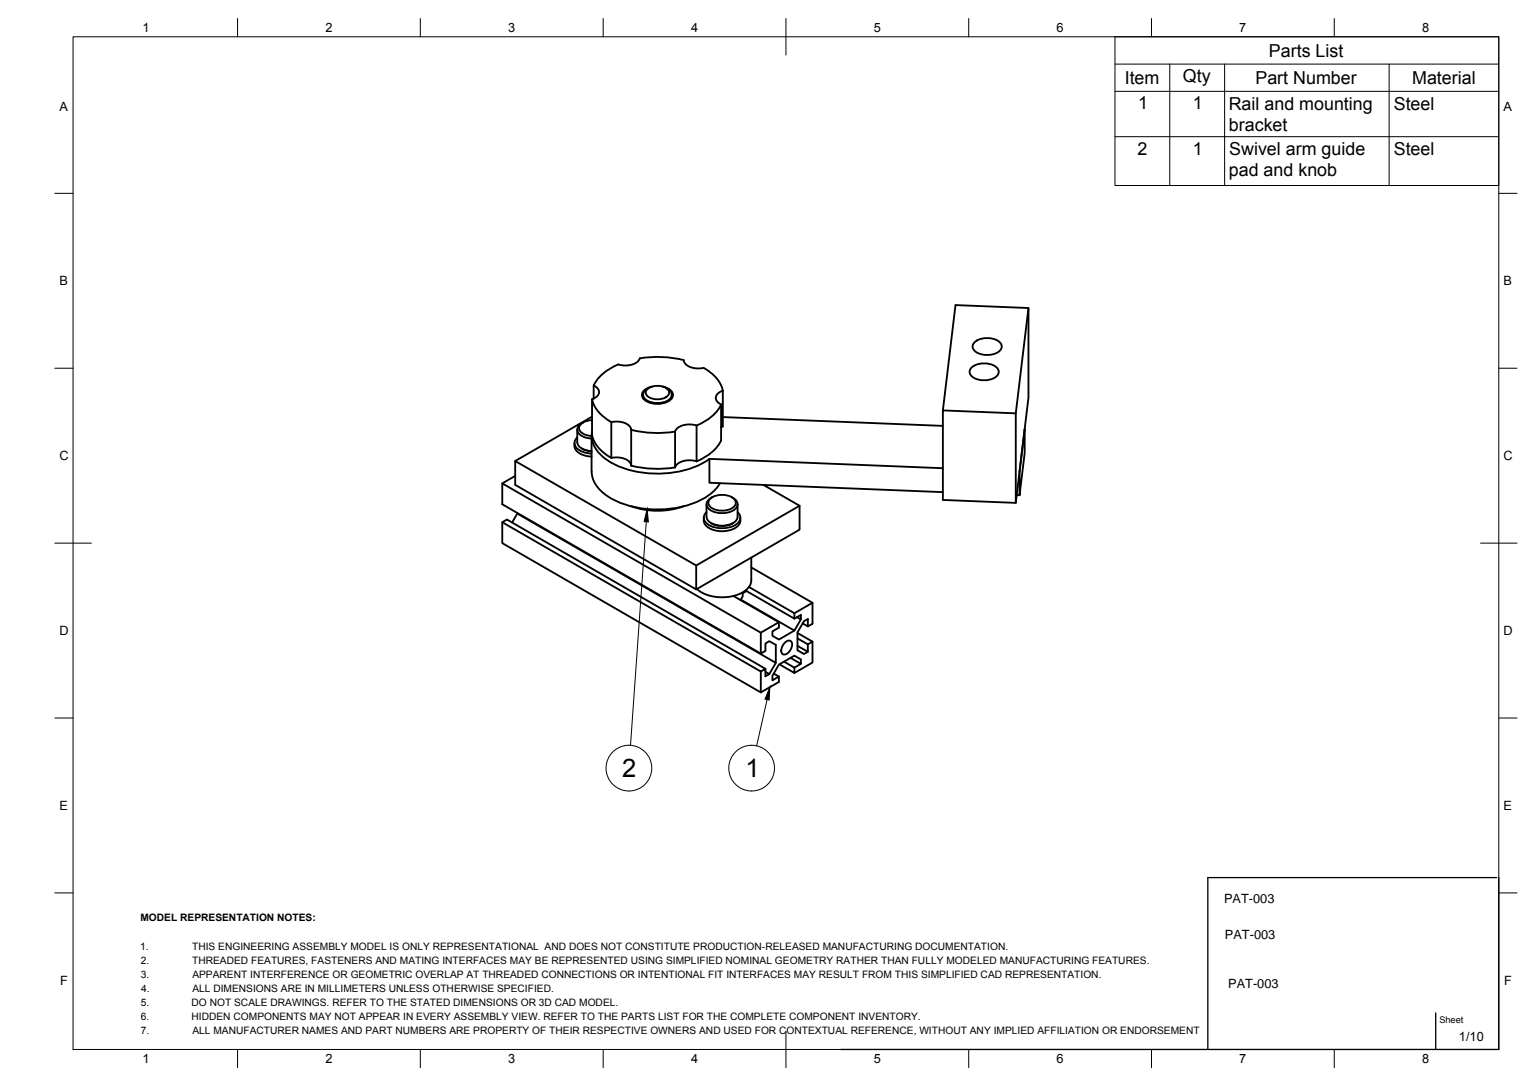
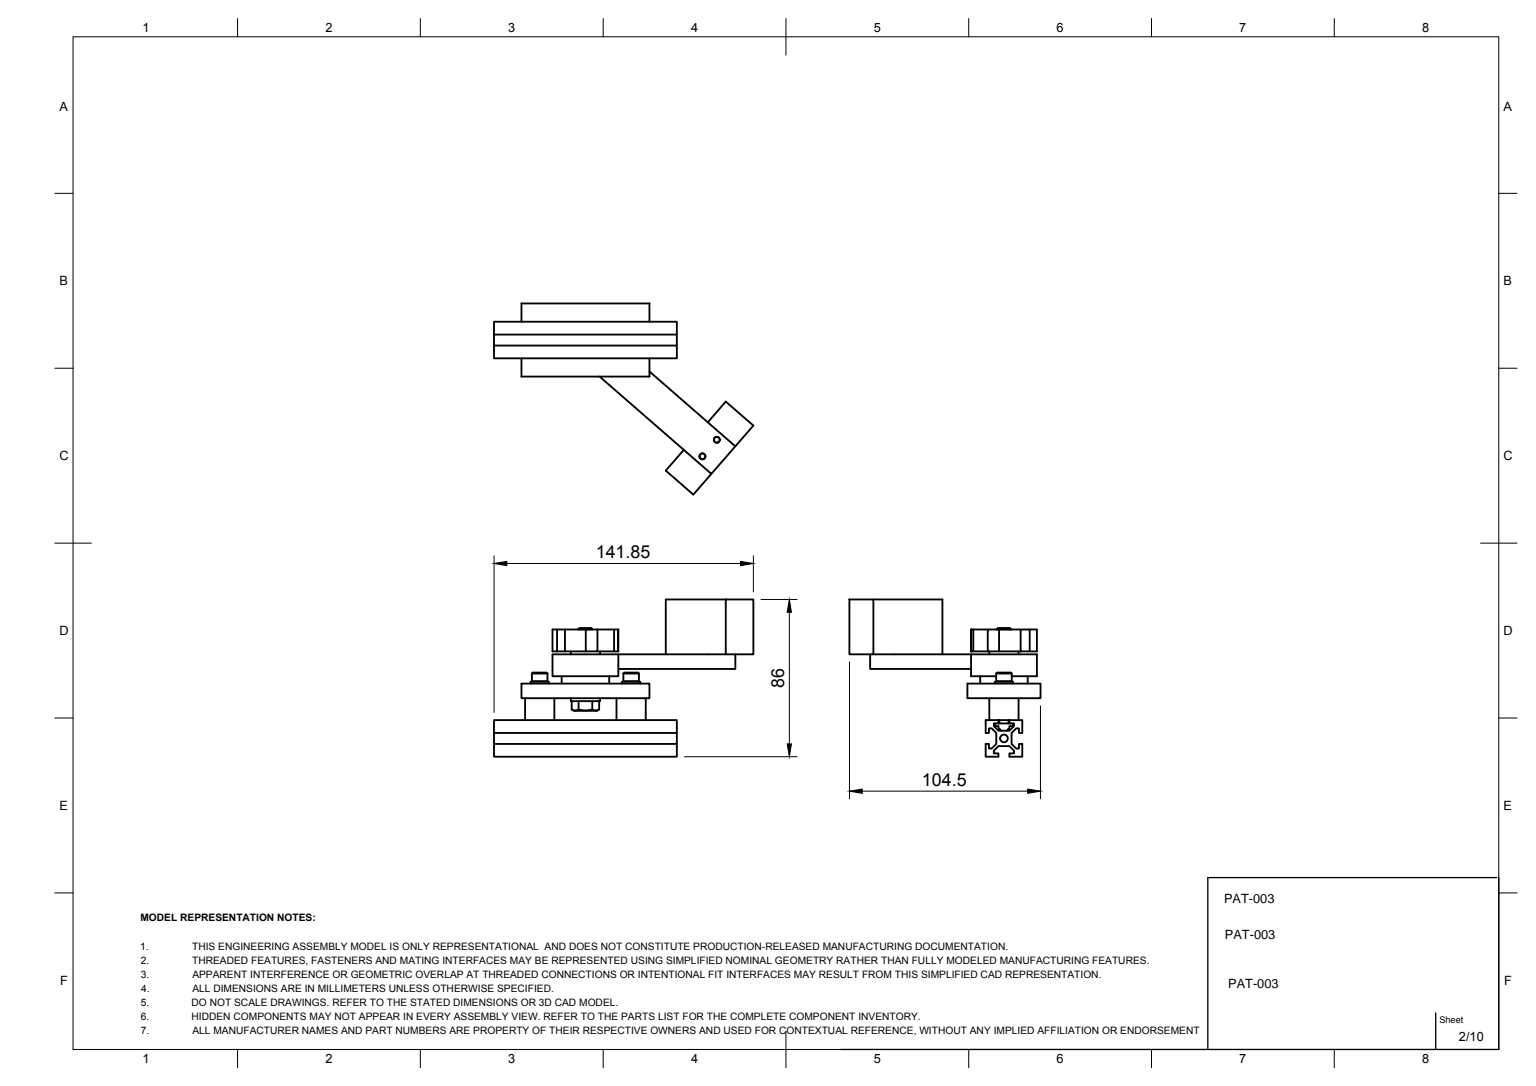
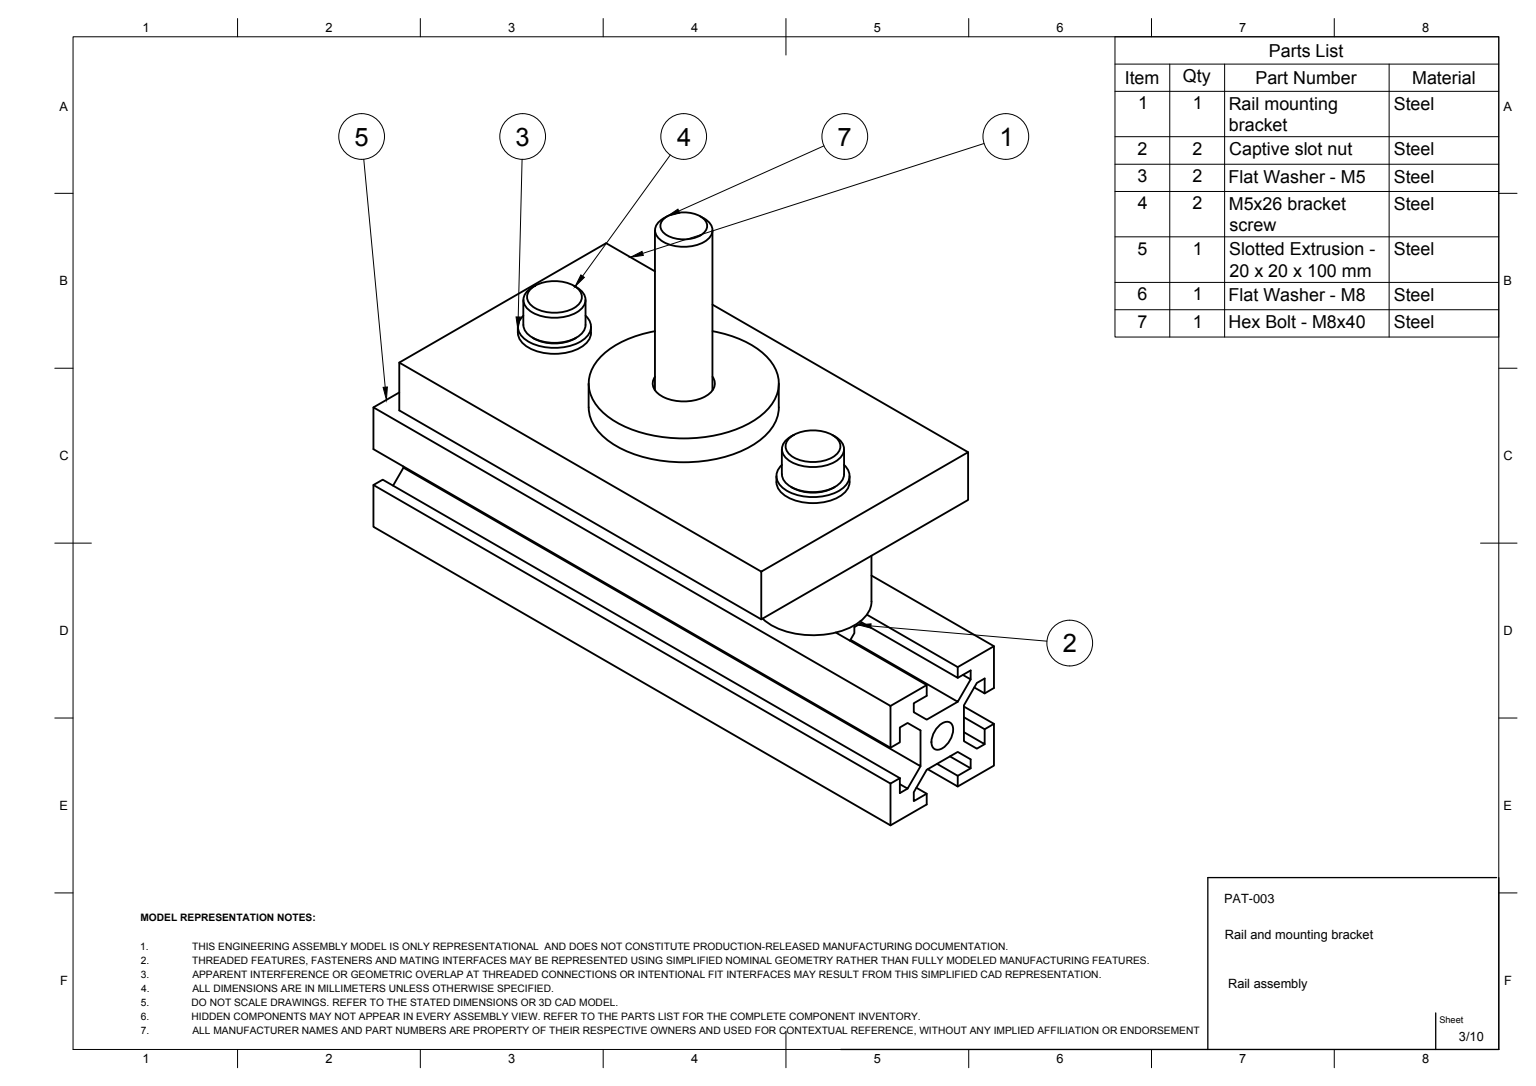
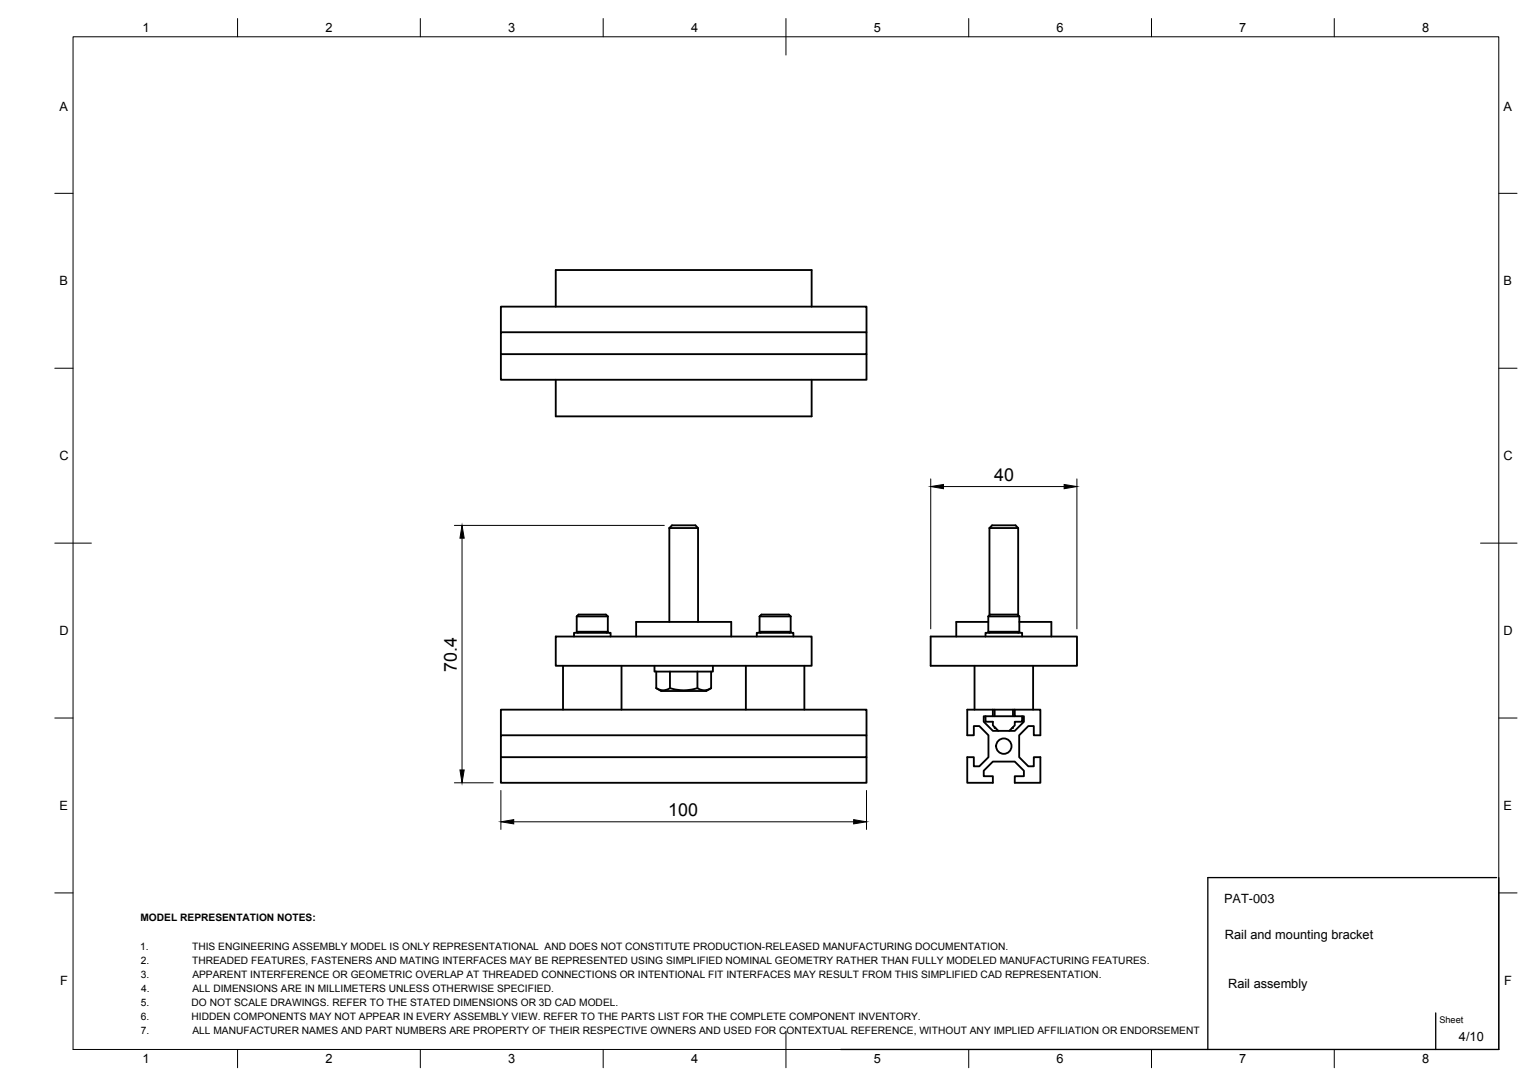
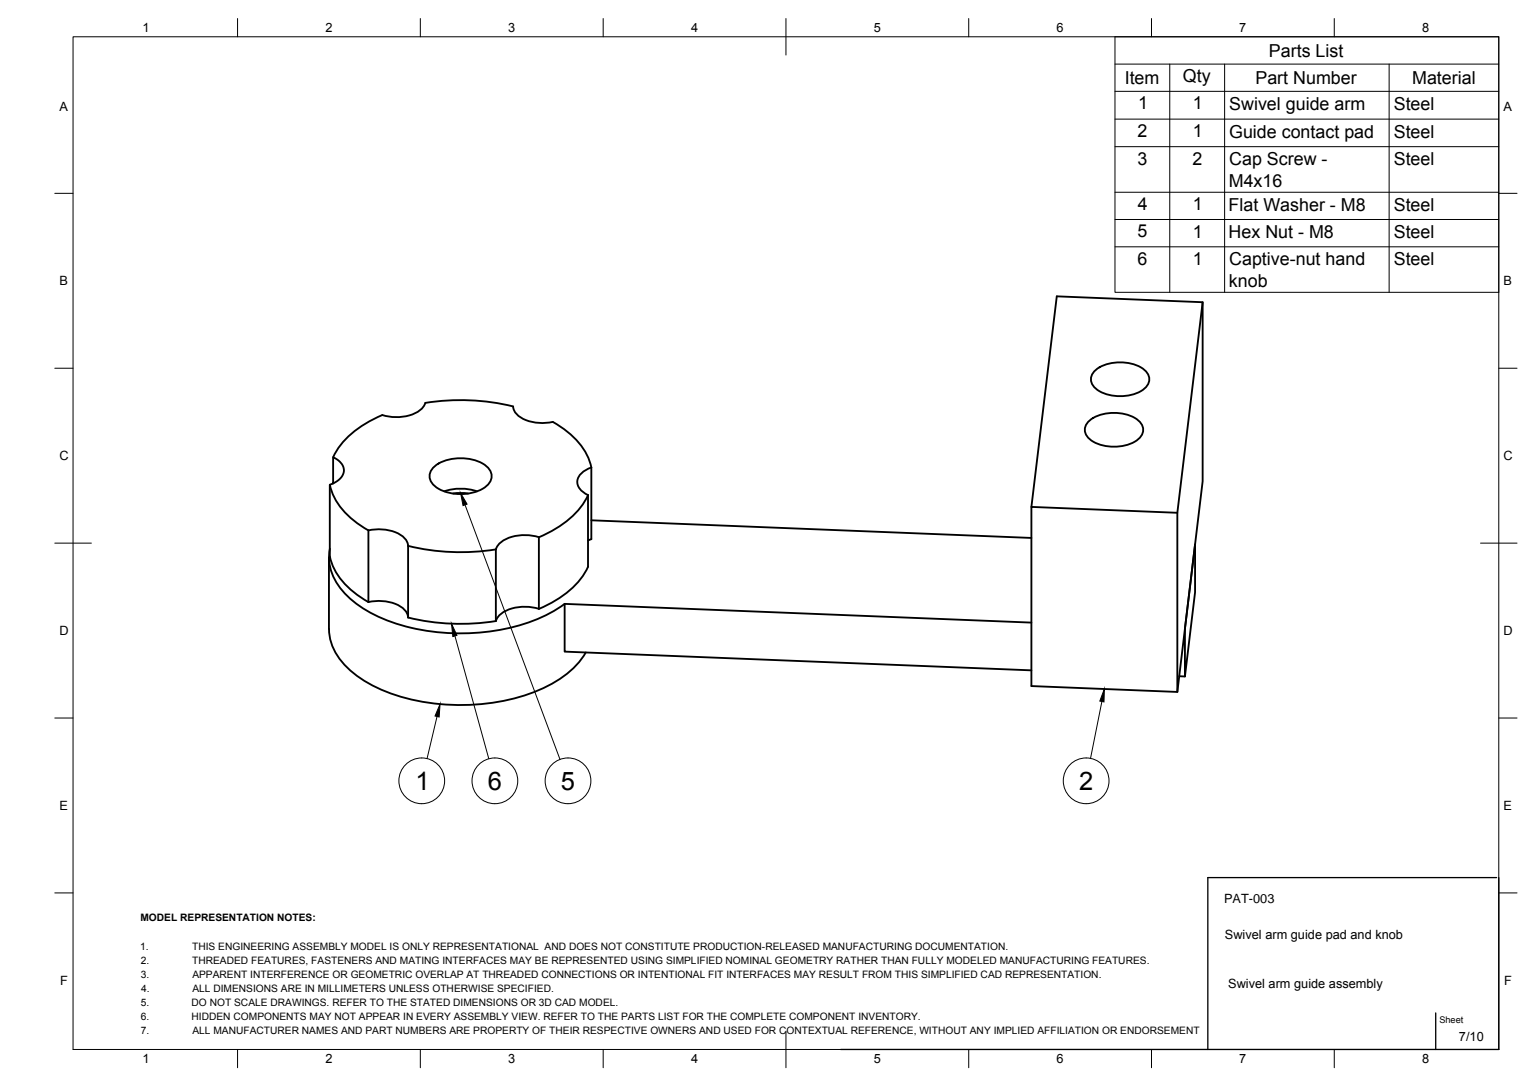
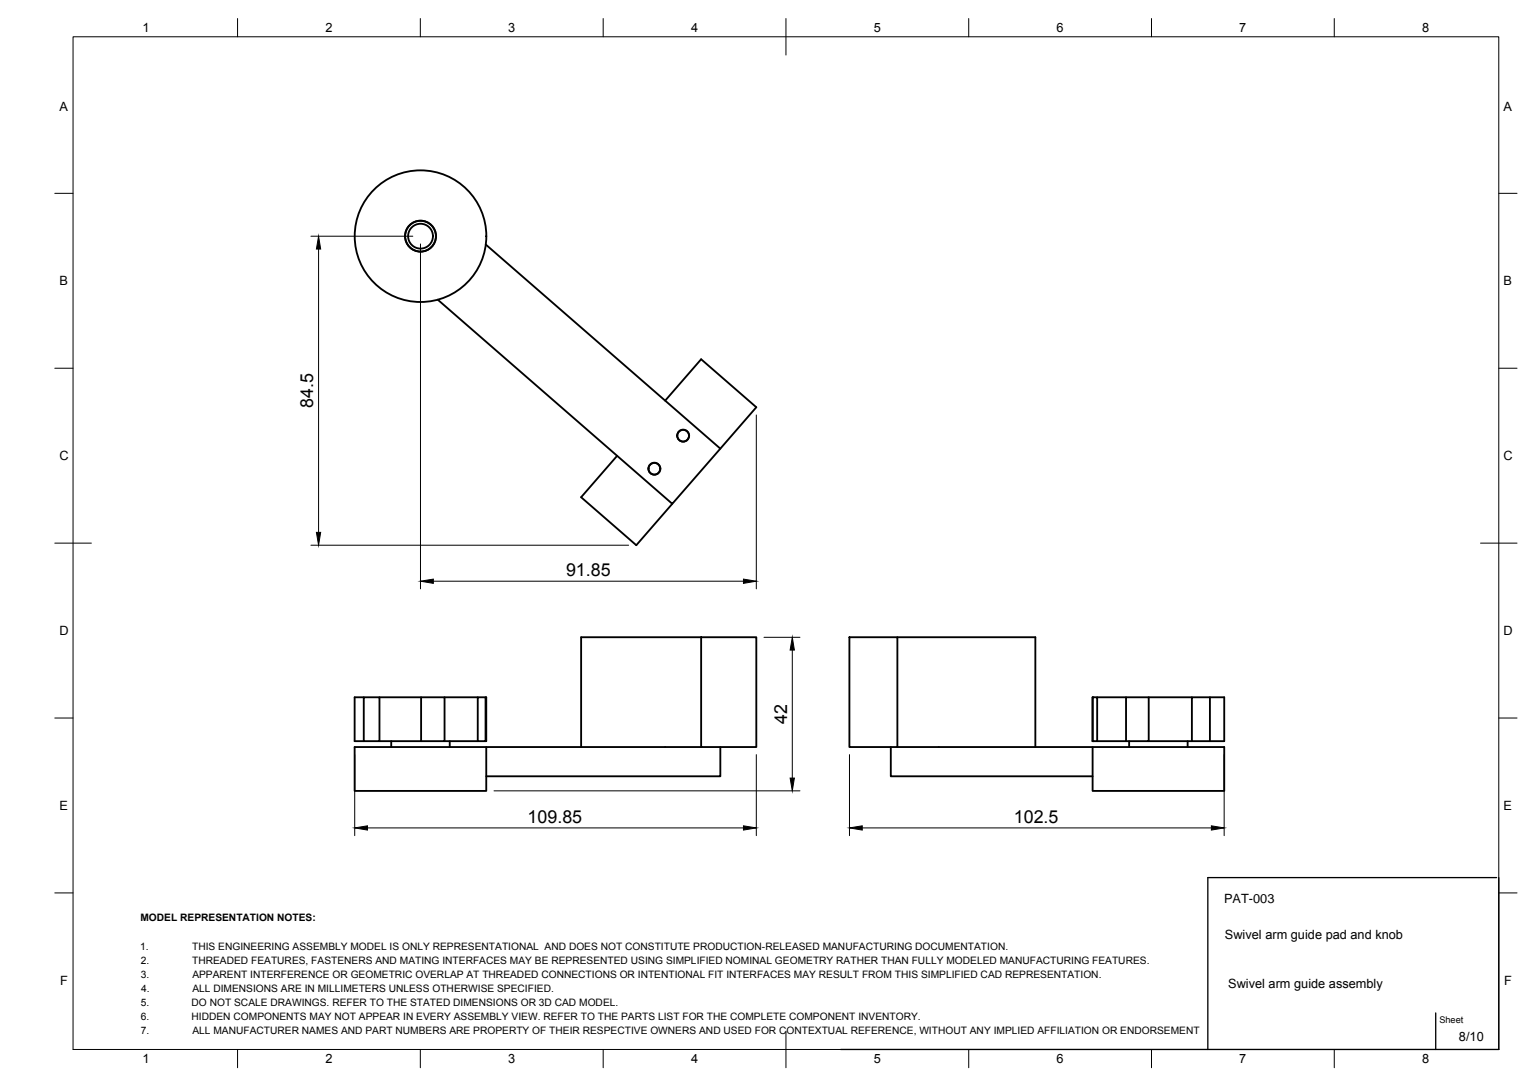
ISO-10303-21;
HEADER;
/* Generated by software containing ST-Developer
 * from STEP Tools, Inc. (www.steptools.com) 
 */

FILE_DESCRIPTION(
/* description */ ('PAT-003'),
/* implementation_level */ '2;1');

FILE_NAME(
/* name */ 'PAT-003',
/* time_stamp */ '2026-10-29T15:45:40-07:00',
/* author */ (''),
/* organization */ (''),
/* preprocessor_version */ 'ST-DEVELOPER v20.2',
/* originating_system */ 'Autodesk Translation Framework v15.17.0.0',
/* authorisation */ '');

FILE_SCHEMA (('AUTOMOTIVE_DESIGN { 1 0 10303 214 3 1 1 }'));
ENDSEC;

DATA;
#10=MECHANICAL_DESIGN_GEOMETRIC_PRESENTATION_REPRESENTATION('',(#147,#148,
#149,#150,#151,#152,#153,#154,#155,#156,#157,#158),#5761);
#11=ITEM_DEFINED_TRANSFORMATION($,$,#3470,#3703);
#12=ITEM_DEFINED_TRANSFORMATION($,$,#3498,#3704);
#13=ITEM_DEFINED_TRANSFORMATION($,$,#3519,#3705);
#14=ITEM_DEFINED_TRANSFORMATION($,$,#3530,#3706);
#15=ITEM_DEFINED_TRANSFORMATION($,$,#3498,#3707);
#16=ITEM_DEFINED_TRANSFORMATION($,$,#3519,#3708);
#17=ITEM_DEFINED_TRANSFORMATION($,$,#3530,#3709);
#18=ITEM_DEFINED_TRANSFORMATION($,$,#3558,#3710);
#19=ITEM_DEFINED_TRANSFORMATION($,$,#3694,#3711);
#20=ITEM_DEFINED_TRANSFORMATION($,$,#3608,#3712);
#21=ITEM_DEFINED_TRANSFORMATION($,$,#3626,#3778);
#22=ITEM_DEFINED_TRANSFORMATION($,$,#3647,#3779);
#23=ITEM_DEFINED_TRANSFORMATION($,$,#3668,#3780);
#24=ITEM_DEFINED_TRANSFORMATION($,$,#3668,#3781);
#25=ITEM_DEFINED_TRANSFORMATION($,$,#3694,#3782);
#26=ITEM_DEFINED_TRANSFORMATION($,$,#3713,#3783);
#27=ITEM_DEFINED_TRANSFORMATION($,$,#3729,#3784);
#28=ITEM_DEFINED_TRANSFORMATION($,$,#3469,#3785);
#29=ITEM_DEFINED_TRANSFORMATION($,$,#3625,#3786);
#30=(
REPRESENTATION_RELATIONSHIP($,$,#5817,#5816)
REPRESENTATION_RELATIONSHIP_WITH_TRANSFORMATION(#11)
SHAPE_REPRESENTATION_RELATIONSHIP()
);
#31=(
REPRESENTATION_RELATIONSHIP($,$,#5818,#5816)
REPRESENTATION_RELATIONSHIP_WITH_TRANSFORMATION(#12)
SHAPE_REPRESENTATION_RELATIONSHIP()
);
#32=(
REPRESENTATION_RELATIONSHIP($,$,#5819,#5816)
REPRESENTATION_RELATIONSHIP_WITH_TRANSFORMATION(#13)
SHAPE_REPRESENTATION_RELATIONSHIP()
);
#33=(
REPRESENTATION_RELATIONSHIP($,$,#5820,#5816)
REPRESENTATION_RELATIONSHIP_WITH_TRANSFORMATION(#14)
SHAPE_REPRESENTATION_RELATIONSHIP()
);
#34=(
REPRESENTATION_RELATIONSHIP($,$,#5818,#5816)
REPRESENTATION_RELATIONSHIP_WITH_TRANSFORMATION(#15)
SHAPE_REPRESENTATION_RELATIONSHIP()
);
#35=(
REPRESENTATION_RELATIONSHIP($,$,#5819,#5816)
REPRESENTATION_RELATIONSHIP_WITH_TRANSFORMATION(#16)
SHAPE_REPRESENTATION_RELATIONSHIP()
);
#36=(
REPRESENTATION_RELATIONSHIP($,$,#5820,#5816)
REPRESENTATION_RELATIONSHIP_WITH_TRANSFORMATION(#17)
SHAPE_REPRESENTATION_RELATIONSHIP()
);
#37=(
REPRESENTATION_RELATIONSHIP($,$,#5821,#5816)
REPRESENTATION_RELATIONSHIP_WITH_TRANSFORMATION(#18)
SHAPE_REPRESENTATION_RELATIONSHIP()
);
#38=(
REPRESENTATION_RELATIONSHIP($,$,#5827,#5816)
REPRESENTATION_RELATIONSHIP_WITH_TRANSFORMATION(#19)
SHAPE_REPRESENTATION_RELATIONSHIP()
);
#39=(
REPRESENTATION_RELATIONSHIP($,$,#5822,#5816)
REPRESENTATION_RELATIONSHIP_WITH_TRANSFORMATION(#20)
SHAPE_REPRESENTATION_RELATIONSHIP()
);
#40=(
REPRESENTATION_RELATIONSHIP($,$,#5824,#5823)
REPRESENTATION_RELATIONSHIP_WITH_TRANSFORMATION(#21)
SHAPE_REPRESENTATION_RELATIONSHIP()
);
#41=(
REPRESENTATION_RELATIONSHIP($,$,#5825,#5823)
REPRESENTATION_RELATIONSHIP_WITH_TRANSFORMATION(#22)
SHAPE_REPRESENTATION_RELATIONSHIP()
);
#42=(
REPRESENTATION_RELATIONSHIP($,$,#5826,#5823)
REPRESENTATION_RELATIONSHIP_WITH_TRANSFORMATION(#23)
SHAPE_REPRESENTATION_RELATIONSHIP()
);
#43=(
REPRESENTATION_RELATIONSHIP($,$,#5826,#5823)
REPRESENTATION_RELATIONSHIP_WITH_TRANSFORMATION(#24)
SHAPE_REPRESENTATION_RELATIONSHIP()
);
#44=(
REPRESENTATION_RELATIONSHIP($,$,#5827,#5823)
REPRESENTATION_RELATIONSHIP_WITH_TRANSFORMATION(#25)
SHAPE_REPRESENTATION_RELATIONSHIP()
);
#45=(
REPRESENTATION_RELATIONSHIP($,$,#5828,#5823)
REPRESENTATION_RELATIONSHIP_WITH_TRANSFORMATION(#26)
SHAPE_REPRESENTATION_RELATIONSHIP()
);
#46=(
REPRESENTATION_RELATIONSHIP($,$,#5829,#5823)
REPRESENTATION_RELATIONSHIP_WITH_TRANSFORMATION(#27)
SHAPE_REPRESENTATION_RELATIONSHIP()
);
#47=(
REPRESENTATION_RELATIONSHIP($,$,#5816,#5815)
REPRESENTATION_RELATIONSHIP_WITH_TRANSFORMATION(#28)
SHAPE_REPRESENTATION_RELATIONSHIP()
);
#48=(
REPRESENTATION_RELATIONSHIP($,$,#5823,#5815)
REPRESENTATION_RELATIONSHIP_WITH_TRANSFORMATION(#29)
SHAPE_REPRESENTATION_RELATIONSHIP()
);
#49=CONTEXT_DEPENDENT_SHAPE_REPRESENTATION(#30,#5794);
#50=CONTEXT_DEPENDENT_SHAPE_REPRESENTATION(#31,#5795);
#51=CONTEXT_DEPENDENT_SHAPE_REPRESENTATION(#32,#5796);
#52=CONTEXT_DEPENDENT_SHAPE_REPRESENTATION(#33,#5797);
#53=CONTEXT_DEPENDENT_SHAPE_REPRESENTATION(#34,#5798);
#54=CONTEXT_DEPENDENT_SHAPE_REPRESENTATION(#35,#5799);
#55=CONTEXT_DEPENDENT_SHAPE_REPRESENTATION(#36,#5800);
#56=CONTEXT_DEPENDENT_SHAPE_REPRESENTATION(#37,#5801);
#57=CONTEXT_DEPENDENT_SHAPE_REPRESENTATION(#38,#5802);
#58=CONTEXT_DEPENDENT_SHAPE_REPRESENTATION(#39,#5803);
#59=CONTEXT_DEPENDENT_SHAPE_REPRESENTATION(#40,#5806);
#60=CONTEXT_DEPENDENT_SHAPE_REPRESENTATION(#41,#5807);
#61=CONTEXT_DEPENDENT_SHAPE_REPRESENTATION(#42,#5808);
#62=CONTEXT_DEPENDENT_SHAPE_REPRESENTATION(#43,#5809);
#63=CONTEXT_DEPENDENT_SHAPE_REPRESENTATION(#44,#5810);
#64=CONTEXT_DEPENDENT_SHAPE_REPRESENTATION(#45,#5811);
#65=CONTEXT_DEPENDENT_SHAPE_REPRESENTATION(#46,#5812);
#66=CONTEXT_DEPENDENT_SHAPE_REPRESENTATION(#47,#5813);
#67=CONTEXT_DEPENDENT_SHAPE_REPRESENTATION(#48,#5814);
#68=NEXT_ASSEMBLY_USAGE_OCCURRENCE('Rail mounting bracket:1',
'Rail mounting bracket:1','Rail mounting bracket:1',#5832,#5833,
'Rail mounting bracket:1');
#69=NEXT_ASSEMBLY_USAGE_OCCURRENCE('Captive slot nut:2',
'Captive slot nut:2','Captive slot nut:2',#5832,#5834,
'Captive slot nut:2');
#70=NEXT_ASSEMBLY_USAGE_OCCURRENCE('Flat Washer - M5:2',
'Flat Washer - M5:2','Flat Washer - M5:2',#5832,#5835,
'Flat Washer - M5:2');
#71=NEXT_ASSEMBLY_USAGE_OCCURRENCE('M5x26 bracket screw:2',
'M5x26 bracket screw:2','M5x26 bracket screw:2',#5832,#5836,
'M5x26 bracket screw:2');
#72=NEXT_ASSEMBLY_USAGE_OCCURRENCE('Captive slot nut:3',
'Captive slot nut:3','Captive slot nut:3',#5832,#5834,
'Captive slot nut:3');
#73=NEXT_ASSEMBLY_USAGE_OCCURRENCE('Flat Washer - M5:3',
'Flat Washer - M5:3','Flat Washer - M5:3',#5832,#5835,
'Flat Washer - M5:3');
#74=NEXT_ASSEMBLY_USAGE_OCCURRENCE('M5x26 bracket screw:3',
'M5x26 bracket screw:3','M5x26 bracket screw:3',#5832,#5836,
'M5x26 bracket screw:3');
#75=NEXT_ASSEMBLY_USAGE_OCCURRENCE(
'Slotted Extrusion - 20 x 20 x 100 mm:2',
'Slotted Extrusion - 20 x 20 x 100 mm:2',
'Slotted Extrusion - 20 x 20 x 100 mm:2',#5832,#5837,
'Slotted Extrusion - 20 x 20 x 100 mm:2');
#76=NEXT_ASSEMBLY_USAGE_OCCURRENCE('Flat Washer - M8:2',
'Flat Washer - M8:2','Flat Washer - M8:2',#5832,#5843,
'Flat Washer - M8:2');
#77=NEXT_ASSEMBLY_USAGE_OCCURRENCE('Hex Bolt - M8x40:2',
'Hex Bolt - M8x40:2','Hex Bolt - M8x40:2',#5832,#5838,
'Hex Bolt - M8x40:2');
#78=NEXT_ASSEMBLY_USAGE_OCCURRENCE('Swivel guide arm:1',
'Swivel guide arm:1','Swivel guide arm:1',#5839,#5840,
'Swivel guide arm:1');
#79=NEXT_ASSEMBLY_USAGE_OCCURRENCE('Guide contact pad:1',
'Guide contact pad:1','Guide contact pad:1',#5839,#5841,
'Guide contact pad:1');
#80=NEXT_ASSEMBLY_USAGE_OCCURRENCE('Cap Screw - M4x16:2',
'Cap Screw - M4x16:2','Cap Screw - M4x16:2',#5839,#5842,
'Cap Screw - M4x16:2');
#81=NEXT_ASSEMBLY_USAGE_OCCURRENCE('Cap Screw - M4x16:3',
'Cap Screw - M4x16:3','Cap Screw - M4x16:3',#5839,#5842,
'Cap Screw - M4x16:3');
#82=NEXT_ASSEMBLY_USAGE_OCCURRENCE('Flat Washer - M8:3',
'Flat Washer - M8:3','Flat Washer - M8:3',#5839,#5843,
'Flat Washer - M8:3');
#83=NEXT_ASSEMBLY_USAGE_OCCURRENCE('Hex Nut - M8:2','Hex Nut - M8:2',
'Hex Nut - M8:2',#5839,#5844,'Hex Nut - M8:2');
#84=NEXT_ASSEMBLY_USAGE_OCCURRENCE('Captive-nut hand knob:2',
'Captive-nut hand knob:2','Captive-nut hand knob:2',#5839,#5845,
'Captive-nut hand knob:2');
#85=NEXT_ASSEMBLY_USAGE_OCCURRENCE('Rail assembly:1','Rail assembly:1',
'Rail assembly:1',#5831,#5832,'Rail assembly:1');
#86=NEXT_ASSEMBLY_USAGE_OCCURRENCE('Swivel arm guide assembly:1',
'Swivel arm guide assembly:1','Swivel arm guide assembly:1',#5831,#5839,
'Swivel arm guide assembly:1');
#87=(
BOUNDED_CURVE()
B_SPLINE_CURVE(2,(#5278,#5279,#5280),.UNSPECIFIED.,.F.,.F.)
B_SPLINE_CURVE_WITH_KNOTS((3,3),(0.14973948338295,0.97160236658079),
 .UNSPECIFIED.)
CURVE()
GEOMETRIC_REPRESENTATION_ITEM()
RATIONAL_B_SPLINE_CURVE((1.07140024848292,1.23714644374248,1.07140024848292))
REPRESENTATION_ITEM('')
);
#88=(
BOUNDED_CURVE()
B_SPLINE_CURVE(2,(#5282,#5283,#5284),.UNSPECIFIED.,.F.,.F.)
B_SPLINE_CURVE_WITH_KNOTS((3,3),(0.14973948338295,0.97160236658079),
 .UNSPECIFIED.)
CURVE()
GEOMETRIC_REPRESENTATION_ITEM()
RATIONAL_B_SPLINE_CURVE((1.07140024848292,1.23714644374248,1.07140024848292))
REPRESENTATION_ITEM('')
);
#89=(
BOUNDED_CURVE()
B_SPLINE_CURVE(2,(#5286,#5287,#5288),.UNSPECIFIED.,.F.,.F.)
B_SPLINE_CURVE_WITH_KNOTS((3,3),(0.14973948338295,0.97160236658079),
 .UNSPECIFIED.)
CURVE()
GEOMETRIC_REPRESENTATION_ITEM()
RATIONAL_B_SPLINE_CURVE((1.07140024848292,1.23714644374248,1.07140024848292))
REPRESENTATION_ITEM('')
);
#90=(
BOUNDED_CURVE()
B_SPLINE_CURVE(2,(#5290,#5291,#5292),.UNSPECIFIED.,.F.,.F.)
B_SPLINE_CURVE_WITH_KNOTS((3,3),(0.149739483382949,0.971602366580789),
 .UNSPECIFIED.)
CURVE()
GEOMETRIC_REPRESENTATION_ITEM()
RATIONAL_B_SPLINE_CURVE((1.07140024848292,1.23714644374248,1.07140024848292))
REPRESENTATION_ITEM('')
);
#91=(
BOUNDED_CURVE()
B_SPLINE_CURVE(2,(#5294,#5295,#5296),.UNSPECIFIED.,.F.,.F.)
B_SPLINE_CURVE_WITH_KNOTS((3,3),(0.14973948338295,0.971602366580789),
 .UNSPECIFIED.)
CURVE()
GEOMETRIC_REPRESENTATION_ITEM()
RATIONAL_B_SPLINE_CURVE((1.07140024848292,1.23714644374248,1.07140024848292))
REPRESENTATION_ITEM('')
);
#92=(
BOUNDED_CURVE()
B_SPLINE_CURVE(2,(#5297,#5298,#5299),.UNSPECIFIED.,.F.,.F.)
B_SPLINE_CURVE_WITH_KNOTS((3,3),(0.14973948338295,0.97160236658079),
 .UNSPECIFIED.)
CURVE()
GEOMETRIC_REPRESENTATION_ITEM()
RATIONAL_B_SPLINE_CURVE((1.07140024848292,1.23714644374248,1.07140024848292))
REPRESENTATION_ITEM('')
);
#93=(
BOUNDED_CURVE()
B_SPLINE_CURVE(2,(#5530,#5531,#5532),.UNSPECIFIED.,.F.,.F.)
B_SPLINE_CURVE_WITH_KNOTS((3,3),(0.14973948338295,0.97160236658079),
 .UNSPECIFIED.)
CURVE()
GEOMETRIC_REPRESENTATION_ITEM()
RATIONAL_B_SPLINE_CURVE((1.07140024848292,1.23714644374248,1.07140024848292))
REPRESENTATION_ITEM('')
);
#94=(
BOUNDED_CURVE()
B_SPLINE_CURVE(2,(#5534,#5535,#5536),.UNSPECIFIED.,.F.,.F.)
B_SPLINE_CURVE_WITH_KNOTS((3,3),(0.14973948338295,0.971602366580789),
 .UNSPECIFIED.)
CURVE()
GEOMETRIC_REPRESENTATION_ITEM()
RATIONAL_B_SPLINE_CURVE((1.07140024848292,1.23714644374248,1.07140024848292))
REPRESENTATION_ITEM('')
);
#95=(
BOUNDED_CURVE()
B_SPLINE_CURVE(2,(#5541,#5542,#5543),.UNSPECIFIED.,.F.,.F.)
B_SPLINE_CURVE_WITH_KNOTS((3,3),(0.14973948338295,0.97160236658079),
 .UNSPECIFIED.)
CURVE()
GEOMETRIC_REPRESENTATION_ITEM()
RATIONAL_B_SPLINE_CURVE((1.07140024848292,1.23714644374248,1.07140024848292))
REPRESENTATION_ITEM('')
);
#96=(
BOUNDED_CURVE()
B_SPLINE_CURVE(2,(#5545,#5546,#5547),.UNSPECIFIED.,.F.,.F.)
B_SPLINE_CURVE_WITH_KNOTS((3,3),(0.14973948338295,0.97160236658079),
 .UNSPECIFIED.)
CURVE()
GEOMETRIC_REPRESENTATION_ITEM()
RATIONAL_B_SPLINE_CURVE((1.07140024848292,1.23714644374248,1.07140024848292))
REPRESENTATION_ITEM('')
);
#97=(
BOUNDED_CURVE()
B_SPLINE_CURVE(2,(#5549,#5550,#5551),.UNSPECIFIED.,.F.,.F.)
B_SPLINE_CURVE_WITH_KNOTS((3,3),(0.14973948338295,0.971602366580789),
 .UNSPECIFIED.)
CURVE()
GEOMETRIC_REPRESENTATION_ITEM()
RATIONAL_B_SPLINE_CURVE((1.07140024848292,1.23714644374248,1.07140024848292))
REPRESENTATION_ITEM('')
);
#98=(
BOUNDED_CURVE()
B_SPLINE_CURVE(2,(#5552,#5553,#5554),.UNSPECIFIED.,.F.,.F.)
B_SPLINE_CURVE_WITH_KNOTS((3,3),(0.14973948338295,0.97160236658079),
 .UNSPECIFIED.)
CURVE()
GEOMETRIC_REPRESENTATION_ITEM()
RATIONAL_B_SPLINE_CURVE((1.07140024848292,1.23714644374248,1.07140024848292))
REPRESENTATION_ITEM('')
);
#99=(
BOUNDED_CURVE()
B_SPLINE_CURVE(2,(#5561,#5562,#5563),.UNSPECIFIED.,.F.,.F.)
B_SPLINE_CURVE_WITH_KNOTS((3,3),(0.14973948338295,0.97160236658079),
 .UNSPECIFIED.)
CURVE()
GEOMETRIC_REPRESENTATION_ITEM()
RATIONAL_B_SPLINE_CURVE((1.07140024848292,1.23714644374248,1.07140024848292))
REPRESENTATION_ITEM('')
);
#100=(
BOUNDED_CURVE()
B_SPLINE_CURVE(2,(#5565,#5566,#5567),.UNSPECIFIED.,.F.,.F.)
B_SPLINE_CURVE_WITH_KNOTS((3,3),(0.14973948338295,0.97160236658079),
 .UNSPECIFIED.)
CURVE()
GEOMETRIC_REPRESENTATION_ITEM()
RATIONAL_B_SPLINE_CURVE((1.07140024848292,1.23714644374248,1.07140024848292))
REPRESENTATION_ITEM('')
);
#101=(
BOUNDED_CURVE()
B_SPLINE_CURVE(2,(#5569,#5570,#5571),.UNSPECIFIED.,.F.,.F.)
B_SPLINE_CURVE_WITH_KNOTS((3,3),(0.14973948338295,0.971602366580789),
 .UNSPECIFIED.)
CURVE()
GEOMETRIC_REPRESENTATION_ITEM()
RATIONAL_B_SPLINE_CURVE((1.07140024848292,1.23714644374248,1.07140024848292))
REPRESENTATION_ITEM('')
);
#102=(
BOUNDED_CURVE()
B_SPLINE_CURVE(2,(#5573,#5574,#5575),.UNSPECIFIED.,.F.,.F.)
B_SPLINE_CURVE_WITH_KNOTS((3,3),(0.14973948338295,0.97160236658079),
 .UNSPECIFIED.)
CURVE()
GEOMETRIC_REPRESENTATION_ITEM()
RATIONAL_B_SPLINE_CURVE((1.07140024848292,1.23714644374248,1.07140024848292))
REPRESENTATION_ITEM('')
);
#103=(
BOUNDED_CURVE()
B_SPLINE_CURVE(2,(#5577,#5578,#5579),.UNSPECIFIED.,.F.,.F.)
B_SPLINE_CURVE_WITH_KNOTS((3,3),(0.14973948338295,0.97160236658079),
 .UNSPECIFIED.)
CURVE()
GEOMETRIC_REPRESENTATION_ITEM()
RATIONAL_B_SPLINE_CURVE((1.07140024848292,1.23714644374248,1.07140024848292))
REPRESENTATION_ITEM('')
);
#104=(
BOUNDED_CURVE()
B_SPLINE_CURVE(2,(#5580,#5581,#5582),.UNSPECIFIED.,.F.,.F.)
B_SPLINE_CURVE_WITH_KNOTS((3,3),(0.14973948338295,0.971602366580789),
 .UNSPECIFIED.)
CURVE()
GEOMETRIC_REPRESENTATION_ITEM()
RATIONAL_B_SPLINE_CURVE((1.07140024848292,1.23714644374248,1.07140024848292))
REPRESENTATION_ITEM('')
);
#105=ORIENTED_CLOSED_SHELL('',*,#3325,.F.);
#106=ORIENTED_CLOSED_SHELL('',*,#3331,.F.);
#107=BREP_WITH_VOIDS('Body1',#3324,(#105));
#108=BREP_WITH_VOIDS('Body1',#3330,(#106));
#109=CONICAL_SURFACE('',#3520,0.275,0.785398163397449);
#110=CONICAL_SURFACE('',#3539,0.4,0.785398163397448);
#111=CONICAL_SURFACE('',#3543,0.41,0.785398163397448);
#112=CONICAL_SURFACE('',#3547,0.26,0.463647609000806);
#113=CONICAL_SURFACE('',#3612,0.36,0.785398163397451);
#114=CONICAL_SURFACE('',#3615,0.734027674973257,1.0471975511966);
#115=CONICAL_SURFACE('',#3671,0.325,0.785398163397448);
#116=CONICAL_SURFACE('',#3675,0.335,0.785398163397448);
#117=CONICAL_SURFACE('',#3679,0.21,0.463647609000806);
#118=CONICAL_SURFACE('',#3683,0.18,0.785398163397448);
#119=CONICAL_SURFACE('',#3714,0.734027674973257,1.0471975511966);
#120=CONICAL_SURFACE('',#3716,0.734027674973257,1.0471975511966);
#121=ELLIPSE('',#3509,0.299389011154384,0.2117);
#122=ELLIPSE('',#3513,0.299389011154384,0.2117);
#123=SHAPE_REPRESENTATION_RELATIONSHIP('SRR','None',#5817,#135);
#124=SHAPE_REPRESENTATION_RELATIONSHIP('SRR','None',#5818,#136);
#125=SHAPE_REPRESENTATION_RELATIONSHIP('SRR','None',#5819,#137);
#126=SHAPE_REPRESENTATION_RELATIONSHIP('SRR','None',#5820,#138);
#127=SHAPE_REPRESENTATION_RELATIONSHIP('SRR','None',#5821,#139);
#128=SHAPE_REPRESENTATION_RELATIONSHIP('SRR','None',#5822,#140);
#129=SHAPE_REPRESENTATION_RELATIONSHIP('SRR','None',#5824,#141);
#130=SHAPE_REPRESENTATION_RELATIONSHIP('SRR','None',#5825,#142);
#131=SHAPE_REPRESENTATION_RELATIONSHIP('SRR','None',#5826,#143);
#132=SHAPE_REPRESENTATION_RELATIONSHIP('SRR','None',#5827,#144);
#133=SHAPE_REPRESENTATION_RELATIONSHIP('SRR','None',#5828,#145);
#134=SHAPE_REPRESENTATION_RELATIONSHIP('SRR','None',#5829,#146);
#135=ADVANCED_BREP_SHAPE_REPRESENTATION('',(#159),#5748);
#136=ADVANCED_BREP_SHAPE_REPRESENTATION('',(#160),#5749);
#137=ADVANCED_BREP_SHAPE_REPRESENTATION('',(#161),#5750);
#138=ADVANCED_BREP_SHAPE_REPRESENTATION('',(#107),#5751);
#139=ADVANCED_BREP_SHAPE_REPRESENTATION('',(#162),#5752);
#140=ADVANCED_BREP_SHAPE_REPRESENTATION('',(#163),#5753);
#141=ADVANCED_BREP_SHAPE_REPRESENTATION('',(#164),#5755);
#142=ADVANCED_BREP_SHAPE_REPRESENTATION('',(#165),#5756);
#143=ADVANCED_BREP_SHAPE_REPRESENTATION('',(#108),#5757);
#144=ADVANCED_BREP_SHAPE_REPRESENTATION('',(#166),#5758);
#145=ADVANCED_BREP_SHAPE_REPRESENTATION('',(#167),#5759);
#146=ADVANCED_BREP_SHAPE_REPRESENTATION('',(#168),#5760);
#147=STYLED_ITEM('',(#5928),#159);
#148=STYLED_ITEM('',(#5956),#160);
#149=STYLED_ITEM('',(#5956),#161);
#150=STYLED_ITEM('',(#5956),#107);
#151=STYLED_ITEM('',(#5963),#162);
#152=STYLED_ITEM('',(#5956),#163);
#153=STYLED_ITEM('',(#5942),#164);
#154=STYLED_ITEM('',(#5942),#165);
#155=STYLED_ITEM('',(#5956),#108);
#156=STYLED_ITEM('',(#5956),#166);
#157=STYLED_ITEM('',(#5956),#167);
#158=STYLED_ITEM('',(#5956),#168);
#159=MANIFOLD_SOLID_BREP('Body1',#3321);
#160=MANIFOLD_SOLID_BREP('Body1',#3322);
#161=MANIFOLD_SOLID_BREP('Body1',#3323);
#162=MANIFOLD_SOLID_BREP('Body1',#3326);
#163=MANIFOLD_SOLID_BREP('Body1',#3327);
#164=MANIFOLD_SOLID_BREP('Body1',#3328);
#165=MANIFOLD_SOLID_BREP('Body1',#3329);
#166=MANIFOLD_SOLID_BREP('Body1',#3332);
#167=MANIFOLD_SOLID_BREP('Body1',#3333);
#168=MANIFOLD_SOLID_BREP('Body1',#3334);
#169=FACE_BOUND('',#530,.T.);
#170=FACE_BOUND('',#533,.T.);
#171=FACE_BOUND('',#539,.T.);
#172=FACE_BOUND('',#545,.T.);
#173=FACE_BOUND('',#546,.T.);
#174=FACE_BOUND('',#547,.T.);
#175=FACE_BOUND('',#549,.T.);
#176=FACE_BOUND('',#550,.T.);
#177=FACE_BOUND('',#551,.T.);
#178=FACE_BOUND('',#555,.T.);
#179=FACE_BOUND('',#570,.T.);
#180=FACE_BOUND('',#573,.T.);
#181=FACE_BOUND('',#575,.T.);
#182=FACE_BOUND('',#583,.T.);
#183=FACE_BOUND('',#640,.T.);
#184=FACE_BOUND('',#642,.T.);
#185=FACE_BOUND('',#655,.T.);
#186=FACE_BOUND('',#659,.T.);
#187=FACE_BOUND('',#660,.T.);
#188=FACE_BOUND('',#661,.T.);
#189=FACE_BOUND('',#666,.T.);
#190=FACE_BOUND('',#667,.T.);
#191=FACE_BOUND('',#671,.T.);
#192=FACE_BOUND('',#674,.T.);
#193=FACE_BOUND('',#677,.T.);
#194=FACE_BOUND('',#685,.T.);
#195=FACE_BOUND('',#686,.T.);
#196=FACE_BOUND('',#688,.T.);
#197=FACE_BOUND('',#689,.T.);
#198=FACE_BOUND('',#695,.T.);
#199=FACE_BOUND('',#711,.T.);
#200=FACE_BOUND('',#713,.T.);
#201=FACE_BOUND('',#724,.T.);
#202=FACE_BOUND('',#726,.T.);
#203=FACE_BOUND('',#734,.T.);
#204=FACE_BOUND('',#748,.T.);
#205=FACE_BOUND('',#751,.T.);
#206=PLANE('',#3474);
#207=PLANE('',#3479);
#208=PLANE('',#3491);
#209=PLANE('',#3492);
#210=PLANE('',#3493);
#211=PLANE('',#3494);
#212=PLANE('',#3495);
#213=PLANE('',#3496);
#214=PLANE('',#3497);
#215=PLANE('',#3499);
#216=PLANE('',#3500);
#217=PLANE('',#3501);
#218=PLANE('',#3503);
#219=PLANE('',#3504);
#220=PLANE('',#3505);
#221=PLANE('',#3506);
#222=PLANE('',#3507);
#223=PLANE('',#3508);
#224=PLANE('',#3515);
#225=PLANE('',#3516);
#226=PLANE('',#3517);
#227=PLANE('',#3518);
#228=PLANE('',#3525);
#229=PLANE('',#3529);
#230=PLANE('',#3531);
#231=PLANE('',#3536);
#232=PLANE('',#3537);
#233=PLANE('',#3545);
#234=PLANE('',#3550);
#235=PLANE('',#3551);
#236=PLANE('',#3552);
#237=PLANE('',#3553);
#238=PLANE('',#3554);
#239=PLANE('',#3555);
#240=PLANE('',#3556);
#241=PLANE('',#3557);
#242=PLANE('',#3559);
#243=PLANE('',#3560);
#244=PLANE('',#3561);
#245=PLANE('',#3562);
#246=PLANE('',#3563);
#247=PLANE('',#3564);
#248=PLANE('',#3565);
#249=PLANE('',#3566);
#250=PLANE('',#3567);
#251=PLANE('',#3568);
#252=PLANE('',#3569);
#253=PLANE('',#3570);
#254=PLANE('',#3571);
#255=PLANE('',#3572);
#256=PLANE('',#3573);
#257=PLANE('',#3574);
#258=PLANE('',#3575);
#259=PLANE('',#3576);
#260=PLANE('',#3577);
#261=PLANE('',#3578);
#262=PLANE('',#3579);
#263=PLANE('',#3580);
#264=PLANE('',#3581);
#265=PLANE('',#3582);
#266=PLANE('',#3583);
#267=PLANE('',#3584);
#268=PLANE('',#3585);
#269=PLANE('',#3586);
#270=PLANE('',#3587);
#271=PLANE('',#3588);
#272=PLANE('',#3589);
#273=PLANE('',#3590);
#274=PLANE('',#3591);
#275=PLANE('',#3592);
#276=PLANE('',#3593);
#277=PLANE('',#3594);
#278=PLANE('',#3598);
#279=PLANE('',#3599);
#280=PLANE('',#3600);
#281=PLANE('',#3601);
#282=PLANE('',#3602);
#283=PLANE('',#3603);
#284=PLANE('',#3604);
#285=PLANE('',#3605);
#286=PLANE('',#3606);
#287=PLANE('',#3607);
#288=PLANE('',#3614);
#289=PLANE('',#3617);
#290=PLANE('',#3618);
#291=PLANE('',#3619);
#292=PLANE('',#3620);
#293=PLANE('',#3621);
#294=PLANE('',#3622);
#295=PLANE('',#3623);
#296=PLANE('',#3624);
#297=PLANE('',#3633);
#298=PLANE('',#3637);
#299=PLANE('',#3638);
#300=PLANE('',#3639);
#301=PLANE('',#3640);
#302=PLANE('',#3646);
#303=PLANE('',#3651);
#304=PLANE('',#3656);
#305=PLANE('',#3662);
#306=PLANE('',#3663);
#307=PLANE('',#3664);
#308=PLANE('',#3665);
#309=PLANE('',#3666);
#310=PLANE('',#3667);
#311=PLANE('',#3669);
#312=PLANE('',#3677);
#313=PLANE('',#3685);
#314=PLANE('',#3686);
#315=PLANE('',#3687);
#316=PLANE('',#3688);
#317=PLANE('',#3689);
#318=PLANE('',#3690);
#319=PLANE('',#3691);
#320=PLANE('',#3692);
#321=PLANE('',#3693);
#322=PLANE('',#3701);
#323=PLANE('',#3702);
#324=PLANE('',#3718);
#325=PLANE('',#3719);
#326=PLANE('',#3720);
#327=PLANE('',#3724);
#328=PLANE('',#3725);
#329=PLANE('',#3726);
#330=PLANE('',#3727);
#331=PLANE('',#3728);
#332=PLANE('',#3748);
#333=PLANE('',#3768);
#334=PLANE('',#3769);
#335=PLANE('',#3770);
#336=PLANE('',#3771);
#337=PLANE('',#3772);
#338=PLANE('',#3773);
#339=PLANE('',#3774);
#340=PLANE('',#3777);
#341=FACE_OUTER_BOUND('',#528,.T.);
#342=FACE_OUTER_BOUND('',#529,.T.);
#343=FACE_OUTER_BOUND('',#531,.T.);
#344=FACE_OUTER_BOUND('',#532,.T.);
#345=FACE_OUTER_BOUND('',#534,.T.);
#346=FACE_OUTER_BOUND('',#535,.T.);
#347=FACE_OUTER_BOUND('',#536,.T.);
#348=FACE_OUTER_BOUND('',#537,.T.);
#349=FACE_OUTER_BOUND('',#538,.T.);
#350=FACE_OUTER_BOUND('',#540,.T.);
#351=FACE_OUTER_BOUND('',#541,.T.);
#352=FACE_OUTER_BOUND('',#542,.T.);
#353=FACE_OUTER_BOUND('',#543,.T.);
#354=FACE_OUTER_BOUND('',#544,.T.);
#355=FACE_OUTER_BOUND('',#548,.T.);
#356=FACE_OUTER_BOUND('',#552,.T.);
#357=FACE_OUTER_BOUND('',#553,.T.);
#358=FACE_OUTER_BOUND('',#554,.T.);
#359=FACE_OUTER_BOUND('',#556,.T.);
#360=FACE_OUTER_BOUND('',#557,.T.);
#361=FACE_OUTER_BOUND('',#558,.T.);
#362=FACE_OUTER_BOUND('',#559,.T.);
#363=FACE_OUTER_BOUND('',#560,.T.);
#364=FACE_OUTER_BOUND('',#561,.T.);
#365=FACE_OUTER_BOUND('',#562,.T.);
#366=FACE_OUTER_BOUND('',#563,.T.);
#367=FACE_OUTER_BOUND('',#564,.T.);
#368=FACE_OUTER_BOUND('',#565,.T.);
#369=FACE_OUTER_BOUND('',#566,.T.);
#370=FACE_OUTER_BOUND('',#567,.T.);
#371=FACE_OUTER_BOUND('',#568,.T.);
#372=FACE_OUTER_BOUND('',#569,.T.);
#373=FACE_OUTER_BOUND('',#571,.T.);
#374=FACE_OUTER_BOUND('',#572,.T.);
#375=FACE_OUTER_BOUND('',#574,.T.);
#376=FACE_OUTER_BOUND('',#576,.T.);
#377=FACE_OUTER_BOUND('',#577,.T.);
#378=FACE_OUTER_BOUND('',#578,.T.);
#379=FACE_OUTER_BOUND('',#579,.T.);
#380=FACE_OUTER_BOUND('',#580,.T.);
#381=FACE_OUTER_BOUND('',#581,.T.);
#382=FACE_OUTER_BOUND('',#582,.T.);
#383=FACE_OUTER_BOUND('',#584,.T.);
#384=FACE_OUTER_BOUND('',#585,.T.);
#385=FACE_OUTER_BOUND('',#586,.T.);
#386=FACE_OUTER_BOUND('',#587,.T.);
#387=FACE_OUTER_BOUND('',#588,.T.);
#388=FACE_OUTER_BOUND('',#589,.T.);
#389=FACE_OUTER_BOUND('',#590,.T.);
#390=FACE_OUTER_BOUND('',#591,.T.);
#391=FACE_OUTER_BOUND('',#592,.T.);
#392=FACE_OUTER_BOUND('',#593,.T.);
#393=FACE_OUTER_BOUND('',#594,.T.);
#394=FACE_OUTER_BOUND('',#595,.T.);
#395=FACE_OUTER_BOUND('',#596,.T.);
#396=FACE_OUTER_BOUND('',#597,.T.);
#397=FACE_OUTER_BOUND('',#598,.T.);
#398=FACE_OUTER_BOUND('',#599,.T.);
#399=FACE_OUTER_BOUND('',#600,.T.);
#400=FACE_OUTER_BOUND('',#601,.T.);
#401=FACE_OUTER_BOUND('',#602,.T.);
#402=FACE_OUTER_BOUND('',#603,.T.);
#403=FACE_OUTER_BOUND('',#604,.T.);
#404=FACE_OUTER_BOUND('',#605,.T.);
#405=FACE_OUTER_BOUND('',#606,.T.);
#406=FACE_OUTER_BOUND('',#607,.T.);
#407=FACE_OUTER_BOUND('',#608,.T.);
#408=FACE_OUTER_BOUND('',#609,.T.);
#409=FACE_OUTER_BOUND('',#610,.T.);
#410=FACE_OUTER_BOUND('',#611,.T.);
#411=FACE_OUTER_BOUND('',#612,.T.);
#412=FACE_OUTER_BOUND('',#613,.T.);
#413=FACE_OUTER_BOUND('',#614,.T.);
#414=FACE_OUTER_BOUND('',#615,.T.);
#415=FACE_OUTER_BOUND('',#616,.T.);
#416=FACE_OUTER_BOUND('',#617,.T.);
#417=FACE_OUTER_BOUND('',#618,.T.);
#418=FACE_OUTER_BOUND('',#619,.T.);
#419=FACE_OUTER_BOUND('',#620,.T.);
#420=FACE_OUTER_BOUND('',#621,.T.);
#421=FACE_OUTER_BOUND('',#622,.T.);
#422=FACE_OUTER_BOUND('',#623,.T.);
#423=FACE_OUTER_BOUND('',#624,.T.);
#424=FACE_OUTER_BOUND('',#625,.T.);
#425=FACE_OUTER_BOUND('',#626,.T.);
#426=FACE_OUTER_BOUND('',#627,.T.);
#427=FACE_OUTER_BOUND('',#628,.T.);
#428=FACE_OUTER_BOUND('',#629,.T.);
#429=FACE_OUTER_BOUND('',#630,.T.);
#430=FACE_OUTER_BOUND('',#631,.T.);
#431=FACE_OUTER_BOUND('',#632,.T.);
#432=FACE_OUTER_BOUND('',#633,.T.);
#433=FACE_OUTER_BOUND('',#634,.T.);
#434=FACE_OUTER_BOUND('',#635,.T.);
#435=FACE_OUTER_BOUND('',#636,.T.);
#436=FACE_OUTER_BOUND('',#637,.T.);
#437=FACE_OUTER_BOUND('',#638,.T.);
#438=FACE_OUTER_BOUND('',#639,.T.);
#439=FACE_OUTER_BOUND('',#641,.T.);
#440=FACE_OUTER_BOUND('',#643,.T.);
#441=FACE_OUTER_BOUND('',#644,.T.);
#442=FACE_OUTER_BOUND('',#645,.T.);
#443=FACE_OUTER_BOUND('',#646,.T.);
#444=FACE_OUTER_BOUND('',#647,.T.);
#445=FACE_OUTER_BOUND('',#648,.T.);
#446=FACE_OUTER_BOUND('',#649,.T.);
#447=FACE_OUTER_BOUND('',#650,.T.);
#448=FACE_OUTER_BOUND('',#651,.T.);
#449=FACE_OUTER_BOUND('',#652,.T.);
#450=FACE_OUTER_BOUND('',#653,.T.);
#451=FACE_OUTER_BOUND('',#654,.T.);
#452=FACE_OUTER_BOUND('',#656,.T.);
#453=FACE_OUTER_BOUND('',#657,.T.);
#454=FACE_OUTER_BOUND('',#658,.T.);
#455=FACE_OUTER_BOUND('',#662,.T.);
#456=FACE_OUTER_BOUND('',#663,.T.);
#457=FACE_OUTER_BOUND('',#664,.T.);
#458=FACE_OUTER_BOUND('',#665,.T.);
#459=FACE_OUTER_BOUND('',#668,.T.);
#460=FACE_OUTER_BOUND('',#669,.T.);
#461=FACE_OUTER_BOUND('',#670,.T.);
#462=FACE_OUTER_BOUND('',#672,.T.);
#463=FACE_OUTER_BOUND('',#673,.T.);
#464=FACE_OUTER_BOUND('',#675,.T.);
#465=FACE_OUTER_BOUND('',#676,.T.);
#466=FACE_OUTER_BOUND('',#678,.T.);
#467=FACE_OUTER_BOUND('',#679,.T.);
#468=FACE_OUTER_BOUND('',#680,.T.);
#469=FACE_OUTER_BOUND('',#681,.T.);
#470=FACE_OUTER_BOUND('',#682,.T.);
#471=FACE_OUTER_BOUND('',#683,.T.);
#472=FACE_OUTER_BOUND('',#684,.T.);
#473=FACE_OUTER_BOUND('',#687,.T.);
#474=FACE_OUTER_BOUND('',#690,.T.);
#475=FACE_OUTER_BOUND('',#691,.T.);
#476=FACE_OUTER_BOUND('',#692,.T.);
#477=FACE_OUTER_BOUND('',#693,.T.);
#478=FACE_OUTER_BOUND('',#694,.T.);
#479=FACE_OUTER_BOUND('',#696,.T.);
#480=FACE_OUTER_BOUND('',#697,.T.);
#481=FACE_OUTER_BOUND('',#698,.T.);
#482=FACE_OUTER_BOUND('',#699,.T.);
#483=FACE_OUTER_BOUND('',#700,.T.);
#484=FACE_OUTER_BOUND('',#701,.T.);
#485=FACE_OUTER_BOUND('',#702,.T.);
#486=FACE_OUTER_BOUND('',#703,.T.);
#487=FACE_OUTER_BOUND('',#704,.T.);
#488=FACE_OUTER_BOUND('',#705,.T.);
#489=FACE_OUTER_BOUND('',#706,.T.);
#490=FACE_OUTER_BOUND('',#707,.T.);
#491=FACE_OUTER_BOUND('',#708,.T.);
#492=FACE_OUTER_BOUND('',#709,.T.);
#493=FACE_OUTER_BOUND('',#710,.T.);
#494=FACE_OUTER_BOUND('',#712,.T.);
#495=FACE_OUTER_BOUND('',#714,.T.);
#496=FACE_OUTER_BOUND('',#715,.T.);
#497=FACE_OUTER_BOUND('',#716,.T.);
#498=FACE_OUTER_BOUND('',#717,.T.);
#499=FACE_OUTER_BOUND('',#718,.T.);
#500=FACE_OUTER_BOUND('',#719,.T.);
#501=FACE_OUTER_BOUND('',#720,.T.);
#502=FACE_OUTER_BOUND('',#721,.T.);
#503=FACE_OUTER_BOUND('',#722,.T.);
#504=FACE_OUTER_BOUND('',#723,.T.);
#505=FACE_OUTER_BOUND('',#725,.T.);
#506=FACE_OUTER_BOUND('',#727,.T.);
#507=FACE_OUTER_BOUND('',#728,.T.);
#508=FACE_OUTER_BOUND('',#729,.T.);
#509=FACE_OUTER_BOUND('',#730,.T.);
#510=FACE_OUTER_BOUND('',#731,.T.);
#511=FACE_OUTER_BOUND('',#732,.T.);
#512=FACE_OUTER_BOUND('',#733,.T.);
#513=FACE_OUTER_BOUND('',#735,.T.);
#514=FACE_OUTER_BOUND('',#736,.T.);
#515=FACE_OUTER_BOUND('',#737,.T.);
#516=FACE_OUTER_BOUND('',#738,.T.);
#517=FACE_OUTER_BOUND('',#739,.T.);
#518=FACE_OUTER_BOUND('',#740,.T.);
#519=FACE_OUTER_BOUND('',#741,.T.);
#520=FACE_OUTER_BOUND('',#742,.T.);
#521=FACE_OUTER_BOUND('',#743,.T.);
#522=FACE_OUTER_BOUND('',#744,.T.);
#523=FACE_OUTER_BOUND('',#745,.T.);
#524=FACE_OUTER_BOUND('',#746,.T.);
#525=FACE_OUTER_BOUND('',#747,.T.);
#526=FACE_OUTER_BOUND('',#749,.T.);
#527=FACE_OUTER_BOUND('',#750,.T.);
#528=EDGE_LOOP('',(#2218,#2219,#2220,#2221));
#529=EDGE_LOOP('',(#2222));
#530=EDGE_LOOP('',(#2223));
#531=EDGE_LOOP('',(#2224,#2225,#2226,#2227));
#532=EDGE_LOOP('',(#2228));
#533=EDGE_LOOP('',(#2229));
#534=EDGE_LOOP('',(#2230,#2231,#2232,#2233));
#535=EDGE_LOOP('',(#2234,#2235,#2236,#2237));
#536=EDGE_LOOP('',(#2238,#2239,#2240,#2241));
#537=EDGE_LOOP('',(#2242,#2243,#2244,#2245));
#538=EDGE_LOOP('',(#2246));
#539=EDGE_LOOP('',(#2247));
#540=EDGE_LOOP('',(#2248,#2249,#2250,#2251));
#541=EDGE_LOOP('',(#2252,#2253,#2254,#2255));
#542=EDGE_LOOP('',(#2256,#2257,#2258,#2259));
#543=EDGE_LOOP('',(#2260,#2261,#2262,#2263));
#544=EDGE_LOOP('',(#2264,#2265,#2266,#2267));
#545=EDGE_LOOP('',(#2268));
#546=EDGE_LOOP('',(#2269));
#547=EDGE_LOOP('',(#2270));
#548=EDGE_LOOP('',(#2271,#2272,#2273,#2274));
#549=EDGE_LOOP('',(#2275));
#550=EDGE_LOOP('',(#2276));
#551=EDGE_LOOP('',(#2277));
#552=EDGE_LOOP('',(#2278,#2279,#2280,#2281));
#553=EDGE_LOOP('',(#2282,#2283,#2284,#2285));
#554=EDGE_LOOP('',(#2286,#2287,#2288,#2289));
#555=EDGE_LOOP('',(#2290));
#556=EDGE_LOOP('',(#2291,#2292,#2293,#2294,#2295,#2296,#2297,#2298,#2299,
#2300));
#557=EDGE_LOOP('',(#2301,#2302,#2303,#2304));
#558=EDGE_LOOP('',(#2305,#2306,#2307,#2308));
#559=EDGE_LOOP('',(#2309,#2310,#2311,#2312,#2313,#2314,#2315,#2316,#2317,
#2318));
#560=EDGE_LOOP('',(#2319,#2320,#2321,#2322));
#561=EDGE_LOOP('',(#2323,#2324,#2325,#2326,#2327,#2328));
#562=EDGE_LOOP('',(#2329,#2330,#2331,#2332,#2333,#2334,#2335,#2336));
#563=EDGE_LOOP('',(#2337,#2338,#2339,#2340,#2341));
#564=EDGE_LOOP('',(#2342,#2343,#2344,#2345));
#565=EDGE_LOOP('',(#2346,#2347,#2348,#2349,#2350,#2351));
#566=EDGE_LOOP('',(#2352,#2353,#2354,#2355));
#567=EDGE_LOOP('',(#2356,#2357,#2358,#2359));
#568=EDGE_LOOP('',(#2360,#2361,#2362,#2363));
#569=EDGE_LOOP('',(#2364));
#570=EDGE_LOOP('',(#2365));
#571=EDGE_LOOP('',(#2366,#2367,#2368,#2369));
#572=EDGE_LOOP('',(#2370));
#573=EDGE_LOOP('',(#2371));
#574=EDGE_LOOP('',(#2372));
#575=EDGE_LOOP('',(#2373));
#576=EDGE_LOOP('',(#2374,#2375,#2376,#2377));
#577=EDGE_LOOP('',(#2378));
#578=EDGE_LOOP('',(#2379));
#579=EDGE_LOOP('',(#2380,#2381,#2382,#2383));
#580=EDGE_LOOP('',(#2384,#2385,#2386,#2387));
#581=EDGE_LOOP('',(#2388,#2389,#2390,#2391));
#582=EDGE_LOOP('',(#2392));
#583=EDGE_LOOP('',(#2393));
#584=EDGE_LOOP('',(#2394,#2395,#2396,#2397));
#585=EDGE_LOOP('',(#2398,#2399,#2400,#2401));
#586=EDGE_LOOP('',(#2402,#2403,#2404,#2405));
#587=EDGE_LOOP('',(#2406,#2407,#2408,#2409));
#588=EDGE_LOOP('',(#2410,#2411,#2412,#2413));
#589=EDGE_LOOP('',(#2414,#2415,#2416,#2417));
#590=EDGE_LOOP('',(#2418,#2419,#2420,#2421));
#591=EDGE_LOOP('',(#2422,#2423,#2424,#2425));
#592=EDGE_LOOP('',(#2426,#2427,#2428,#2429,#2430,#2431));
#593=EDGE_LOOP('',(#2432,#2433,#2434,#2435,#2436,#2437));
#594=EDGE_LOOP('',(#2438,#2439,#2440,#2441));
#595=EDGE_LOOP('',(#2442,#2443,#2444,#2445));
#596=EDGE_LOOP('',(#2446,#2447,#2448,#2449));
#597=EDGE_LOOP('',(#2450,#2451,#2452,#2453));
#598=EDGE_LOOP('',(#2454,#2455,#2456,#2457));
#599=EDGE_LOOP('',(#2458,#2459,#2460,#2461));
#600=EDGE_LOOP('',(#2462,#2463,#2464,#2465));
#601=EDGE_LOOP('',(#2466,#2467,#2468,#2469));
#602=EDGE_LOOP('',(#2470,#2471,#2472,#2473));
#603=EDGE_LOOP('',(#2474,#2475,#2476,#2477));
#604=EDGE_LOOP('',(#2478,#2479,#2480,#2481));
#605=EDGE_LOOP('',(#2482,#2483,#2484,#2485));
#606=EDGE_LOOP('',(#2486,#2487,#2488,#2489));
#607=EDGE_LOOP('',(#2490,#2491,#2492,#2493));
#608=EDGE_LOOP('',(#2494,#2495,#2496,#2497));
#609=EDGE_LOOP('',(#2498,#2499,#2500,#2501));
#610=EDGE_LOOP('',(#2502,#2503,#2504,#2505));
#611=EDGE_LOOP('',(#2506,#2507,#2508,#2509));
#612=EDGE_LOOP('',(#2510,#2511,#2512,#2513));
#613=EDGE_LOOP('',(#2514,#2515,#2516,#2517));
#614=EDGE_LOOP('',(#2518,#2519,#2520,#2521));
#615=EDGE_LOOP('',(#2522,#2523,#2524,#2525));
#616=EDGE_LOOP('',(#2526,#2527,#2528,#2529));
#617=EDGE_LOOP('',(#2530,#2531,#2532,#2533));
#618=EDGE_LOOP('',(#2534,#2535,#2536,#2537));
#619=EDGE_LOOP('',(#2538,#2539,#2540,#2541));
#620=EDGE_LOOP('',(#2542,#2543,#2544,#2545));
#621=EDGE_LOOP('',(#2546,#2547,#2548,#2549));
#622=EDGE_LOOP('',(#2550,#2551,#2552,#2553));
#623=EDGE_LOOP('',(#2554,#2555,#2556,#2557));
#624=EDGE_LOOP('',(#2558,#2559,#2560,#2561));
#625=EDGE_LOOP('',(#2562,#2563,#2564,#2565));
#626=EDGE_LOOP('',(#2566,#2567,#2568,#2569));
#627=EDGE_LOOP('',(#2570,#2571,#2572,#2573));
#628=EDGE_LOOP('',(#2574,#2575,#2576,#2577));
#629=EDGE_LOOP('',(#2578,#2579,#2580,#2581));
#630=EDGE_LOOP('',(#2582,#2583,#2584,#2585));
#631=EDGE_LOOP('',(#2586,#2587,#2588,#2589));
#632=EDGE_LOOP('',(#2590,#2591,#2592,#2593));
#633=EDGE_LOOP('',(#2594,#2595,#2596,#2597));
#634=EDGE_LOOP('',(#2598,#2599,#2600,#2601));
#635=EDGE_LOOP('',(#2602,#2603,#2604,#2605));
#636=EDGE_LOOP('',(#2606,#2607,#2608,#2609));
#637=EDGE_LOOP('',(#2610,#2611,#2612,#2613));
#638=EDGE_LOOP('',(#2614,#2615,#2616,#2617));
#639=EDGE_LOOP('',(#2618,#2619,#2620,#2621,#2622,#2623,#2624,#2625,#2626,
#2627,#2628,#2629,#2630,#2631,#2632,#2633,#2634,#2635,#2636,#2637,#2638,
#2639,#2640,#2641,#2642,#2643,#2644,#2645,#2646,#2647,#2648,#2649,#2650,
#2651,#2652,#2653,#2654,#2655,#2656,#2657,#2658,#2659,#2660,#2661));
#640=EDGE_LOOP('',(#2662));
#641=EDGE_LOOP('',(#2663,#2664,#2665,#2666,#2667,#2668,#2669,#2670,#2671,
#2672,#2673,#2674,#2675,#2676,#2677,#2678,#2679,#2680,#2681,#2682,#2683,
#2684,#2685,#2686,#2687,#2688,#2689,#2690,#2691,#2692,#2693,#2694,#2695,
#2696,#2697,#2698,#2699,#2700,#2701,#2702,#2703,#2704,#2705,#2706));
#642=EDGE_LOOP('',(#2707));
#643=EDGE_LOOP('',(#2708,#2709,#2710,#2711));
#644=EDGE_LOOP('',(#2712,#2713,#2714,#2715));
#645=EDGE_LOOP('',(#2716));
#646=EDGE_LOOP('',(#2717,#2718,#2719,#2720,#2721,#2722,#2723,#2724,#2725));
#647=EDGE_LOOP('',(#2726,#2727,#2728,#2729));
#648=EDGE_LOOP('',(#2730,#2731,#2732,#2733));
#649=EDGE_LOOP('',(#2734,#2735,#2736,#2737));
#650=EDGE_LOOP('',(#2738,#2739,#2740,#2741));
#651=EDGE_LOOP('',(#2742,#2743,#2744,#2745));
#652=EDGE_LOOP('',(#2746,#2747,#2748,#2749));
#653=EDGE_LOOP('',(#2750));
#654=EDGE_LOOP('',(#2751,#2752,#2753,#2754,#2755,#2756));
#655=EDGE_LOOP('',(#2757));
#656=EDGE_LOOP('',(#2758,#2759,#2760,#2761));
#657=EDGE_LOOP('',(#2762,#2763,#2764,#2765));
#658=EDGE_LOOP('',(#2766,#2767,#2768,#2769,#2770));
#659=EDGE_LOOP('',(#2771));
#660=EDGE_LOOP('',(#2772));
#661=EDGE_LOOP('',(#2773));
#662=EDGE_LOOP('',(#2774,#2775,#2776,#2777));
#663=EDGE_LOOP('',(#2778,#2779,#2780,#2781));
#664=EDGE_LOOP('',(#2782,#2783,#2784,#2785));
#665=EDGE_LOOP('',(#2786,#2787,#2788,#2789));
#666=EDGE_LOOP('',(#2790));
#667=EDGE_LOOP('',(#2791));
#668=EDGE_LOOP('',(#2792,#2793,#2794,#2795,#2796,#2797,#2798,#2799));
#669=EDGE_LOOP('',(#2800,#2801,#2802,#2803));
#670=EDGE_LOOP('',(#2804));
#671=EDGE_LOOP('',(#2805));
#672=EDGE_LOOP('',(#2806,#2807,#2808,#2809));
#673=EDGE_LOOP('',(#2810));
#674=EDGE_LOOP('',(#2811));
#675=EDGE_LOOP('',(#2812,#2813,#2814,#2815));
#676=EDGE_LOOP('',(#2816));
#677=EDGE_LOOP('',(#2817));
#678=EDGE_LOOP('',(#2818,#2819,#2820,#2821));
#679=EDGE_LOOP('',(#2822,#2823,#2824,#2825));
#680=EDGE_LOOP('',(#2826,#2827,#2828,#2829));
#681=EDGE_LOOP('',(#2830,#2831,#2832,#2833));
#682=EDGE_LOOP('',(#2834,#2835,#2836,#2837));
#683=EDGE_LOOP('',(#2838,#2839,#2840,#2841));
#684=EDGE_LOOP('',(#2842,#2843,#2844,#2845));
#685=EDGE_LOOP('',(#2846));
#686=EDGE_LOOP('',(#2847));
#687=EDGE_LOOP('',(#2848,#2849,#2850,#2851));
#688=EDGE_LOOP('',(#2852));
#689=EDGE_LOOP('',(#2853));
#690=EDGE_LOOP('',(#2854));
#691=EDGE_LOOP('',(#2855,#2856,#2857,#2858));
#692=EDGE_LOOP('',(#2859,#2860,#2861,#2862));
#693=EDGE_LOOP('',(#2863,#2864,#2865,#2866));
#694=EDGE_LOOP('',(#2867));
#695=EDGE_LOOP('',(#2868));
#696=EDGE_LOOP('',(#2869,#2870,#2871,#2872));
#697=EDGE_LOOP('',(#2873,#2874,#2875,#2876));
#698=EDGE_LOOP('',(#2877,#2878,#2879,#2880));
#699=EDGE_LOOP('',(#2881));
#700=EDGE_LOOP('',(#2882,#2883,#2884,#2885));
#701=EDGE_LOOP('',(#2886,#2887,#2888,#2889));
#702=EDGE_LOOP('',(#2890,#2891,#2892,#2893));
#703=EDGE_LOOP('',(#2894,#2895,#2896,#2897));
#704=EDGE_LOOP('',(#2898,#2899,#2900,#2901));
#705=EDGE_LOOP('',(#2902,#2903,#2904,#2905));
#706=EDGE_LOOP('',(#2906,#2907,#2908,#2909,#2910,#2911));
#707=EDGE_LOOP('',(#2912,#2913,#2914,#2915,#2916,#2917));
#708=EDGE_LOOP('',(#2918,#2919,#2920,#2921));
#709=EDGE_LOOP('',(#2922,#2923,#2924,#2925));
#710=EDGE_LOOP('',(#2926));
#711=EDGE_LOOP('',(#2927));
#712=EDGE_LOOP('',(#2928));
#713=EDGE_LOOP('',(#2929));
#714=EDGE_LOOP('',(#2930,#2931,#2932,#2933,#2934,#2935,#2936,#2937,#2938));
#715=EDGE_LOOP('',(#2939,#2940,#2941,#2942,#2943,#2944,#2945,#2946,#2947));
#716=EDGE_LOOP('',(#2948,#2949,#2950,#2951));
#717=EDGE_LOOP('',(#2952,#2953,#2954,#2955));
#718=EDGE_LOOP('',(#2956,#2957,#2958,#2959));
#719=EDGE_LOOP('',(#2960,#2961,#2962,#2963));
#720=EDGE_LOOP('',(#2964,#2965,#2966,#2967));
#721=EDGE_LOOP('',(#2968,#2969,#2970,#2971));
#722=EDGE_LOOP('',(#2972,#2973,#2974,#2975));
#723=EDGE_LOOP('',(#2976));
#724=EDGE_LOOP('',(#2977));
#725=EDGE_LOOP('',(#2978));
#726=EDGE_LOOP('',(#2979));
#727=EDGE_LOOP('',(#2980,#2981,#2982,#2983));
#728=EDGE_LOOP('',(#2984,#2985,#2986,#2987));
#729=EDGE_LOOP('',(#2988,#2989,#2990,#2991));
#730=EDGE_LOOP('',(#2992,#2993,#2994,#2995));
#731=EDGE_LOOP('',(#2996,#2997,#2998,#2999));
#732=EDGE_LOOP('',(#3000,#3001,#3002,#3003));
#733=EDGE_LOOP('',(#3004,#3005,#3006,#3007,#3008,#3009,#3010,#3011,#3012,
#3013,#3014,#3015));
#734=EDGE_LOOP('',(#3016));
#735=EDGE_LOOP('',(#3017,#3018,#3019,#3020));
#736=EDGE_LOOP('',(#3021,#3022,#3023,#3024));
#737=EDGE_LOOP('',(#3025,#3026,#3027,#3028));
#738=EDGE_LOOP('',(#3029,#3030,#3031,#3032));
#739=EDGE_LOOP('',(#3033,#3034,#3035,#3036));
#740=EDGE_LOOP('',(#3037,#3038,#3039,#3040));
#741=EDGE_LOOP('',(#3041,#3042,#3043,#3044));
#742=EDGE_LOOP('',(#3045,#3046,#3047,#3048));
#743=EDGE_LOOP('',(#3049,#3050,#3051,#3052));
#744=EDGE_LOOP('',(#3053,#3054,#3055,#3056));
#745=EDGE_LOOP('',(#3057,#3058,#3059,#3060));
#746=EDGE_LOOP('',(#3061,#3062,#3063,#3064));
#747=EDGE_LOOP('',(#3065,#3066,#3067,#3068,#3069,#3070));
#748=EDGE_LOOP('',(#3071));
#749=EDGE_LOOP('',(#3072,#3073,#3074,#3075));
#750=EDGE_LOOP('',(#3076,#3077,#3078,#3079,#3080,#3081,#3082,#3083,#3084,
#3085,#3086,#3087));
#751=EDGE_LOOP('',(#3088,#3089,#3090,#3091,#3092,#3093));
#752=LINE('',#4754,#1074);
#753=LINE('',#4763,#1075);
#754=LINE('',#4770,#1076);
#755=LINE('',#4774,#1077);
#756=LINE('',#4780,#1078);
#757=LINE('',#4786,#1079);
#758=LINE('',#4792,#1080);
#759=LINE('',#4794,#1081);
#760=LINE('',#4796,#1082);
#761=LINE('',#4797,#1083);
#762=LINE('',#4800,#1084);
#763=LINE('',#4802,#1085);
#764=LINE('',#4803,#1086);
#765=LINE('',#4806,#1087);
#766=LINE('',#4808,#1088);
#767=LINE('',#4809,#1089);
#768=LINE('',#4811,#1090);
#769=LINE('',#4812,#1091);
#770=LINE('',#4819,#1092);
#771=LINE('',#4821,#1093);
#772=LINE('',#4823,#1094);
#773=LINE('',#4824,#1095);
#774=LINE('',#4827,#1096);
#775=LINE('',#4829,#1097);
#776=LINE('',#4830,#1098);
#777=LINE('',#4833,#1099);
#778=LINE('',#4835,#1100);
#779=LINE('',#4836,#1101);
#780=LINE('',#4841,#1102);
#781=LINE('',#4843,#1103);
#782=LINE('',#4845,#1104);
#783=LINE('',#4847,#1105);
#784=LINE('',#4849,#1106);
#785=LINE('',#4851,#1107);
#786=LINE('',#4852,#1108);
#787=LINE('',#4855,#1109);
#788=LINE('',#4856,#1110);
#789=LINE('',#4859,#1111);
#790=LINE('',#4860,#1112);
#791=LINE('',#4863,#1113);
#792=LINE('',#4865,#1114);
#793=LINE('',#4867,#1115);
#794=LINE('',#4869,#1116);
#795=LINE('',#4870,#1117);
#796=LINE('',#4872,#1118);
#797=LINE('',#4875,#1119);
#798=LINE('',#4878,#1120);
#799=LINE('',#4882,#1121);
#800=LINE('',#4889,#1122);
#801=LINE('',#4891,#1123);
#802=LINE('',#4893,#1124);
#803=LINE('',#4900,#1125);
#804=LINE('',#4904,#1126);
#805=LINE('',#4911,#1127);
#806=LINE('',#4922,#1128);
#807=LINE('',#4931,#1129);
#808=LINE('',#4935,#1130);
#809=LINE('',#4939,#1131);
#810=LINE('',#4946,#1132);
#811=LINE('',#4948,#1133);
#812=LINE('',#4952,#1134);
#813=LINE('',#4954,#1135);
#814=LINE('',#4956,#1136);
#815=LINE('',#4957,#1137);
#816=LINE('',#4960,#1138);
#817=LINE('',#4962,#1139);
#818=LINE('',#4963,#1140);
#819=LINE('',#4966,#1141);
#820=LINE('',#4968,#1142);
#821=LINE('',#4969,#1143);
#822=LINE('',#4972,#1144);
#823=LINE('',#4974,#1145);
#824=LINE('',#4975,#1146);
#825=LINE('',#4978,#1147);
#826=LINE('',#4980,#1148);
#827=LINE('',#4981,#1149);
#828=LINE('',#4983,#1150);
#829=LINE('',#4984,#1151);
#830=LINE('',#4991,#1152);
#831=LINE('',#4993,#1153);
#832=LINE('',#4995,#1154);
#833=LINE('',#4996,#1155);
#834=LINE('',#4999,#1156);
#835=LINE('',#5001,#1157);
#836=LINE('',#5002,#1158);
#837=LINE('',#5005,#1159);
#838=LINE('',#5007,#1160);
#839=LINE('',#5008,#1161);
#840=LINE('',#5011,#1162);
#841=LINE('',#5013,#1163);
#842=LINE('',#5014,#1164);
#843=LINE('',#5017,#1165);
#844=LINE('',#5019,#1166);
#845=LINE('',#5020,#1167);
#846=LINE('',#5023,#1168);
#847=LINE('',#5025,#1169);
#848=LINE('',#5026,#1170);
#849=LINE('',#5029,#1171);
#850=LINE('',#5031,#1172);
#851=LINE('',#5032,#1173);
#852=LINE('',#5035,#1174);
#853=LINE('',#5037,#1175);
#854=LINE('',#5038,#1176);
#855=LINE('',#5041,#1177);
#856=LINE('',#5043,#1178);
#857=LINE('',#5044,#1179);
#858=LINE('',#5048,#1180);
#859=LINE('',#5050,#1181);
#860=LINE('',#5052,#1182);
#861=LINE('',#5053,#1183);
#862=LINE('',#5056,#1184);
#863=LINE('',#5058,#1185);
#864=LINE('',#5059,#1186);
#865=LINE('',#5062,#1187);
#866=LINE('',#5064,#1188);
#867=LINE('',#5065,#1189);
#868=LINE('',#5068,#1190);
#869=LINE('',#5070,#1191);
#870=LINE('',#5071,#1192);
#871=LINE('',#5074,#1193);
#872=LINE('',#5076,#1194);
#873=LINE('',#5077,#1195);
#874=LINE('',#5080,#1196);
#875=LINE('',#5082,#1197);
#876=LINE('',#5083,#1198);
#877=LINE('',#5086,#1199);
#878=LINE('',#5088,#1200);
#879=LINE('',#5089,#1201);
#880=LINE('',#5092,#1202);
#881=LINE('',#5094,#1203);
#882=LINE('',#5095,#1204);
#883=LINE('',#5098,#1205);
#884=LINE('',#5100,#1206);
#885=LINE('',#5101,#1207);
#886=LINE('',#5105,#1208);
#887=LINE('',#5107,#1209);
#888=LINE('',#5109,#1210);
#889=LINE('',#5110,#1211);
#890=LINE('',#5113,#1212);
#891=LINE('',#5115,#1213);
#892=LINE('',#5116,#1214);
#893=LINE('',#5119,#1215);
#894=LINE('',#5121,#1216);
#895=LINE('',#5122,#1217);
#896=LINE('',#5125,#1218);
#897=LINE('',#5127,#1219);
#898=LINE('',#5128,#1220);
#899=LINE('',#5131,#1221);
#900=LINE('',#5133,#1222);
#901=LINE('',#5134,#1223);
#902=LINE('',#5137,#1224);
#903=LINE('',#5139,#1225);
#904=LINE('',#5140,#1226);
#905=LINE('',#5143,#1227);
#906=LINE('',#5145,#1228);
#907=LINE('',#5146,#1229);
#908=LINE('',#5149,#1230);
#909=LINE('',#5151,#1231);
#910=LINE('',#5152,#1232);
#911=LINE('',#5155,#1233);
#912=LINE('',#5157,#1234);
#913=LINE('',#5158,#1235);
#914=LINE('',#5162,#1236);
#915=LINE('',#5164,#1237);
#916=LINE('',#5166,#1238);
#917=LINE('',#5167,#1239);
#918=LINE('',#5170,#1240);
#919=LINE('',#5172,#1241);
#920=LINE('',#5173,#1242);
#921=LINE('',#5176,#1243);
#922=LINE('',#5178,#1244);
#923=LINE('',#5179,#1245);
#924=LINE('',#5182,#1246);
#925=LINE('',#5184,#1247);
#926=LINE('',#5185,#1248);
#927=LINE('',#5188,#1249);
#928=LINE('',#5190,#1250);
#929=LINE('',#5191,#1251);
#930=LINE('',#5194,#1252);
#931=LINE('',#5196,#1253);
#932=LINE('',#5197,#1254);
#933=LINE('',#5200,#1255);
#934=LINE('',#5202,#1256);
#935=LINE('',#5203,#1257);
#936=LINE('',#5206,#1258);
#937=LINE('',#5208,#1259);
#938=LINE('',#5209,#1260);
#939=LINE('',#5212,#1261);
#940=LINE('',#5214,#1262);
#941=LINE('',#5215,#1263);
#942=LINE('',#5220,#1264);
#943=LINE('',#5224,#1265);
#944=LINE('',#5226,#1266);
#945=LINE('',#5227,#1267);
#946=LINE('',#5230,#1268);
#947=LINE('',#5232,#1269);
#948=LINE('',#5233,#1270);
#949=LINE('',#5235,#1271);
#950=LINE('',#5236,#1272);
#951=LINE('',#5239,#1273);
#952=LINE('',#5241,#1274);
#953=LINE('',#5242,#1275);
#954=LINE('',#5244,#1276);
#955=LINE('',#5245,#1277);
#956=LINE('',#5248,#1278);
#957=LINE('',#5250,#1279);
#958=LINE('',#5251,#1280);
#959=LINE('',#5253,#1281);
#960=LINE('',#5254,#1282);
#961=LINE('',#5256,#1283);
#962=LINE('',#5257,#1284);
#963=LINE('',#5265,#1285);
#964=LINE('',#5270,#1286);
#965=LINE('',#5276,#1287);
#966=LINE('',#5302,#1288);
#967=LINE('',#5304,#1289);
#968=LINE('',#5305,#1290);
#969=LINE('',#5308,#1291);
#970=LINE('',#5309,#1292);
#971=LINE('',#5312,#1293);
#972=LINE('',#5313,#1294);
#973=LINE('',#5316,#1295);
#974=LINE('',#5317,#1296);
#975=LINE('',#5320,#1297);
#976=LINE('',#5321,#1298);
#977=LINE('',#5323,#1299);
#978=LINE('',#5332,#1300);
#979=LINE('',#5338,#1301);
#980=LINE('',#5347,#1302);
#981=LINE('',#5349,#1303);
#982=LINE('',#5350,#1304);
#983=LINE('',#5355,#1305);
#984=LINE('',#5357,#1306);
#985=LINE('',#5358,#1307);
#986=LINE('',#5361,#1308);
#987=LINE('',#5362,#1309);
#988=LINE('',#5365,#1310);
#989=LINE('',#5366,#1311);
#990=LINE('',#5371,#1312);
#991=LINE('',#5375,#1313);
#992=LINE('',#5383,#1314);
#993=LINE('',#5392,#1315);
#994=LINE('',#5400,#1316);
#995=LINE('',#5404,#1317);
#996=LINE('',#5408,#1318);
#997=LINE('',#5410,#1319);
#998=LINE('',#5412,#1320);
#999=LINE('',#5413,#1321);
#1000=LINE('',#5416,#1322);
#1001=LINE('',#5418,#1323);
#1002=LINE('',#5419,#1324);
#1003=LINE('',#5422,#1325);
#1004=LINE('',#5424,#1326);
#1005=LINE('',#5425,#1327);
#1006=LINE('',#5427,#1328);
#1007=LINE('',#5428,#1329);
#1008=LINE('',#5438,#1330);
#1009=LINE('',#5442,#1331);
#1010=LINE('',#5446,#1332);
#1011=LINE('',#5453,#1333);
#1012=LINE('',#5457,#1334);
#1013=LINE('',#5461,#1335);
#1014=LINE('',#5466,#1336);
#1015=LINE('',#5468,#1337);
#1016=LINE('',#5470,#1338);
#1017=LINE('',#5471,#1339);
#1018=LINE('',#5474,#1340);
#1019=LINE('',#5476,#1341);
#1020=LINE('',#5477,#1342);
#1021=LINE('',#5480,#1343);
#1022=LINE('',#5482,#1344);
#1023=LINE('',#5483,#1345);
#1024=LINE('',#5486,#1346);
#1025=LINE('',#5488,#1347);
#1026=LINE('',#5489,#1348);
#1027=LINE('',#5492,#1349);
#1028=LINE('',#5494,#1350);
#1029=LINE('',#5495,#1351);
#1030=LINE('',#5497,#1352);
#1031=LINE('',#5498,#1353);
#1032=LINE('',#5506,#1354);
#1033=LINE('',#5512,#1355);
#1034=LINE('',#5538,#1356);
#1035=LINE('',#5559,#1357);
#1036=LINE('',#5584,#1358);
#1037=LINE('',#5585,#1359);
#1038=LINE('',#5587,#1360);
#1039=LINE('',#5589,#1361);
#1040=LINE('',#5594,#1362);
#1041=LINE('',#5597,#1363);
#1042=LINE('',#5599,#1364);
#1043=LINE('',#5607,#1365);
#1044=LINE('',#5611,#1366);
#1045=LINE('',#5616,#1367);
#1046=LINE('',#5620,#1368);
#1047=LINE('',#5625,#1369);
#1048=LINE('',#5629,#1370);
#1049=LINE('',#5634,#1371);
#1050=LINE('',#5638,#1372);
#1051=LINE('',#5643,#1373);
#1052=LINE('',#5647,#1374);
#1053=LINE('',#5652,#1375);
#1054=LINE('',#5656,#1376);
#1055=LINE('',#5682,#1377);
#1056=LINE('',#5684,#1378);
#1057=LINE('',#5686,#1379);
#1058=LINE('',#5687,#1380);
#1059=LINE('',#5690,#1381);
#1060=LINE('',#5692,#1382);
#1061=LINE('',#5693,#1383);
#1062=LINE('',#5696,#1384);
#1063=LINE('',#5698,#1385);
#1064=LINE('',#5699,#1386);
#1065=LINE('',#5702,#1387);
#1066=LINE('',#5704,#1388);
#1067=LINE('',#5705,#1389);
#1068=LINE('',#5708,#1390);
#1069=LINE('',#5710,#1391);
#1070=LINE('',#5711,#1392);
#1071=LINE('',#5713,#1393);
#1072=LINE('',#5714,#1394);
#1073=LINE('',#5719,#1395);
#1074=VECTOR('',#3797,0.800000000000001);
#1075=VECTOR('',#3808,0.8);
#1076=VECTOR('',#3817,0.275);
#1077=VECTOR('',#3822,0.275);
#1078=VECTOR('',#3829,0.425);
#1079=VECTOR('',#3836,1.3);
#1080=VECTOR('',#3843,1.);
#1081=VECTOR('',#3844,1.);
#1082=VECTOR('',#3845,1.);
#1083=VECTOR('',#3846,1.);
#1084=VECTOR('',#3849,1.);
#1085=VECTOR('',#3850,1.);
#1086=VECTOR('',#3851,1.);
#1087=VECTOR('',#3854,1.);
#1088=VECTOR('',#3855,1.);
#1089=VECTOR('',#3856,1.);
#1090=VECTOR('',#3859,1.);
#1091=VECTOR('',#3860,1.);
#1092=VECTOR('',#3869,1.);
#1093=VECTOR('',#3870,1.);
#1094=VECTOR('',#3871,1.);
#1095=VECTOR('',#3872,1.);
#1096=VECTOR('',#3875,1.);
#1097=VECTOR('',#3876,1.);
#1098=VECTOR('',#3877,1.);
#1099=VECTOR('',#3880,1.);
#1100=VECTOR('',#3881,1.);
#1101=VECTOR('',#3882,1.);
#1102=VECTOR('',#3887,1.);
#1103=VECTOR('',#3888,1.);
#1104=VECTOR('',#3889,1.);
#1105=VECTOR('',#3890,1.);
#1106=VECTOR('',#3891,1.);
#1107=VECTOR('',#3892,1.);
#1108=VECTOR('',#3893,1.);
#1109=VECTOR('',#3896,1.);
#1110=VECTOR('',#3897,1.);
#1111=VECTOR('',#3900,1.);
#1112=VECTOR('',#3901,1.);
#1113=VECTOR('',#3904,1.);
#1114=VECTOR('',#3905,1.);
#1115=VECTOR('',#3906,1.);
#1116=VECTOR('',#3907,1.);
#1117=VECTOR('',#3908,1.);
#1118=VECTOR('',#3911,1.);
#1119=VECTOR('',#3914,1.);
#1120=VECTOR('',#3917,1.);
#1121=VECTOR('',#3922,0.21);
#1122=VECTOR('',#3931,1.);
#1123=VECTOR('',#3934,1.);
#1124=VECTOR('',#3937,1.);
#1125=VECTOR('',#3946,0.275);
#1126=VECTOR('',#3951,0.265);
#1127=VECTOR('',#3960,0.5);
#1128=VECTOR('',#3975,0.25);
#1129=VECTOR('',#3988,0.4);
#1130=VECTOR('',#3993,0.425);
#1131=VECTOR('',#3998,0.41);
#1132=VECTOR('',#4007,0.26);
#1133=VECTOR('',#4010,0.25);
#1134=VECTOR('',#4013,1.);
#1135=VECTOR('',#4014,1.);
#1136=VECTOR('',#4015,1.);
#1137=VECTOR('',#4016,1.);
#1138=VECTOR('',#4019,1.);
#1139=VECTOR('',#4020,1.);
#1140=VECTOR('',#4021,1.);
#1141=VECTOR('',#4024,1.);
#1142=VECTOR('',#4025,1.);
#1143=VECTOR('',#4026,1.);
#1144=VECTOR('',#4029,1.);
#1145=VECTOR('',#4030,1.);
#1146=VECTOR('',#4031,1.);
#1147=VECTOR('',#4034,1.);
#1148=VECTOR('',#4035,1.);
#1149=VECTOR('',#4036,1.);
#1150=VECTOR('',#4039,1.);
#1151=VECTOR('',#4040,1.);
#1152=VECTOR('',#4049,1.);
#1153=VECTOR('',#4050,1.);
#1154=VECTOR('',#4051,1.);
#1155=VECTOR('',#4052,1.);
#1156=VECTOR('',#4055,1.);
#1157=VECTOR('',#4056,1.);
#1158=VECTOR('',#4057,1.);
#1159=VECTOR('',#4060,1.);
#1160=VECTOR('',#4061,1.);
#1161=VECTOR('',#4062,1.);
#1162=VECTOR('',#4065,1.);
#1163=VECTOR('',#4066,1.);
#1164=VECTOR('',#4067,1.);
#1165=VECTOR('',#4070,1.);
#1166=VECTOR('',#4071,1.);
#1167=VECTOR('',#4072,1.);
#1168=VECTOR('',#4075,1.);
#1169=VECTOR('',#4076,1.);
#1170=VECTOR('',#4077,1.);
#1171=VECTOR('',#4080,1.);
#1172=VECTOR('',#4081,1.);
#1173=VECTOR('',#4082,1.);
#1174=VECTOR('',#4085,1.);
#1175=VECTOR('',#4086,1.);
#1176=VECTOR('',#4087,1.);
#1177=VECTOR('',#4090,1.);
#1178=VECTOR('',#4091,1.);
#1179=VECTOR('',#4092,1.);
#1180=VECTOR('',#4095,1.);
#1181=VECTOR('',#4096,1.);
#1182=VECTOR('',#4097,1.);
#1183=VECTOR('',#4098,1.);
#1184=VECTOR('',#4101,1.);
#1185=VECTOR('',#4102,1.);
#1186=VECTOR('',#4103,1.);
#1187=VECTOR('',#4106,1.);
#1188=VECTOR('',#4107,1.);
#1189=VECTOR('',#4108,1.);
#1190=VECTOR('',#4111,1.);
#1191=VECTOR('',#4112,1.);
#1192=VECTOR('',#4113,1.);
#1193=VECTOR('',#4116,1.);
#1194=VECTOR('',#4117,1.);
#1195=VECTOR('',#4118,1.);
#1196=VECTOR('',#4121,1.);
#1197=VECTOR('',#4122,1.);
#1198=VECTOR('',#4123,1.);
#1199=VECTOR('',#4126,1.);
#1200=VECTOR('',#4127,1.);
#1201=VECTOR('',#4128,1.);
#1202=VECTOR('',#4131,1.);
#1203=VECTOR('',#4132,1.);
#1204=VECTOR('',#4133,1.);
#1205=VECTOR('',#4136,1.);
#1206=VECTOR('',#4137,1.);
#1207=VECTOR('',#4138,1.);
#1208=VECTOR('',#4141,1.);
#1209=VECTOR('',#4142,1.);
#1210=VECTOR('',#4143,1.);
#1211=VECTOR('',#4144,1.);
#1212=VECTOR('',#4147,1.);
#1213=VECTOR('',#4148,1.);
#1214=VECTOR('',#4149,1.);
#1215=VECTOR('',#4152,1.);
#1216=VECTOR('',#4153,1.);
#1217=VECTOR('',#4154,1.);
#1218=VECTOR('',#4157,1.);
#1219=VECTOR('',#4158,1.);
#1220=VECTOR('',#4159,1.);
#1221=VECTOR('',#4162,1.);
#1222=VECTOR('',#4163,1.);
#1223=VECTOR('',#4164,1.);
#1224=VECTOR('',#4167,1.);
#1225=VECTOR('',#4168,1.);
#1226=VECTOR('',#4169,1.);
#1227=VECTOR('',#4172,1.);
#1228=VECTOR('',#4173,1.);
#1229=VECTOR('',#4174,1.);
#1230=VECTOR('',#4177,1.);
#1231=VECTOR('',#4178,1.);
#1232=VECTOR('',#4179,1.);
#1233=VECTOR('',#4182,1.);
#1234=VECTOR('',#4183,1.);
#1235=VECTOR('',#4184,1.);
#1236=VECTOR('',#4187,1.);
#1237=VECTOR('',#4188,1.);
#1238=VECTOR('',#4189,1.);
#1239=VECTOR('',#4190,1.);
#1240=VECTOR('',#4193,1.);
#1241=VECTOR('',#4194,1.);
#1242=VECTOR('',#4195,1.);
#1243=VECTOR('',#4198,1.);
#1244=VECTOR('',#4199,1.);
#1245=VECTOR('',#4200,1.);
#1246=VECTOR('',#4203,1.);
#1247=VECTOR('',#4204,1.);
#1248=VECTOR('',#4205,1.);
#1249=VECTOR('',#4208,1.);
#1250=VECTOR('',#4209,1.);
#1251=VECTOR('',#4210,1.);
#1252=VECTOR('',#4213,1.);
#1253=VECTOR('',#4214,1.);
#1254=VECTOR('',#4215,1.);
#1255=VECTOR('',#4218,1.);
#1256=VECTOR('',#4219,1.);
#1257=VECTOR('',#4220,1.);
#1258=VECTOR('',#4223,1.);
#1259=VECTOR('',#4224,1.);
#1260=VECTOR('',#4225,1.);
#1261=VECTOR('',#4228,1.);
#1262=VECTOR('',#4229,1.);
#1263=VECTOR('',#4230,1.);
#1264=VECTOR('',#4235,0.21);
#1265=VECTOR('',#4240,1.);
#1266=VECTOR('',#4241,1.);
#1267=VECTOR('',#4242,1.);
#1268=VECTOR('',#4245,1.);
#1269=VECTOR('',#4246,1.);
#1270=VECTOR('',#4247,1.);
#1271=VECTOR('',#4250,1.);
#1272=VECTOR('',#4251,1.);
#1273=VECTOR('',#4254,1.);
#1274=VECTOR('',#4255,1.);
#1275=VECTOR('',#4256,1.);
#1276=VECTOR('',#4259,1.);
#1277=VECTOR('',#4260,1.);
#1278=VECTOR('',#4263,1.);
#1279=VECTOR('',#4264,1.);
#1280=VECTOR('',#4265,1.);
#1281=VECTOR('',#4268,1.);
#1282=VECTOR('',#4269,1.);
#1283=VECTOR('',#4272,1.);
#1284=VECTOR('',#4273,1.);
#1285=VECTOR('',#4284,0.4);
#1286=VECTOR('',#4291,0.36);
#1287=VECTOR('',#4298,0.734027674973257);
#1288=VECTOR('',#4301,1.);
#1289=VECTOR('',#4302,1.);
#1290=VECTOR('',#4303,1.);
#1291=VECTOR('',#4306,1.);
#1292=VECTOR('',#4307,1.);
#1293=VECTOR('',#4310,1.);
#1294=VECTOR('',#4311,1.);
#1295=VECTOR('',#4314,1.);
#1296=VECTOR('',#4315,1.);
#1297=VECTOR('',#4318,1.);
#1298=VECTOR('',#4319,1.);
#1299=VECTOR('',#4322,1.);
#1300=VECTOR('',#4335,0.164999999999999);
#1301=VECTOR('',#4342,0.164999999999999);
#1302=VECTOR('',#4351,1.);
#1303=VECTOR('',#4352,1.);
#1304=VECTOR('',#4353,1.);
#1305=VECTOR('',#4358,1.);
#1306=VECTOR('',#4359,1.);
#1307=VECTOR('',#4360,1.);
#1308=VECTOR('',#4363,1.);
#1309=VECTOR('',#4364,1.);
#1310=VECTOR('',#4367,1.);
#1311=VECTOR('',#4368,1.);
#1312=VECTOR('',#4375,1.8);
#1313=VECTOR('',#4380,0.425);
#1314=VECTOR('',#4391,0.4);
#1315=VECTOR('',#4402,0.4);
#1316=VECTOR('',#4413,0.225);
#1317=VECTOR('',#4418,0.225);
#1318=VECTOR('',#4421,1.);
#1319=VECTOR('',#4422,1.);
#1320=VECTOR('',#4423,1.);
#1321=VECTOR('',#4424,1.);
#1322=VECTOR('',#4427,1.);
#1323=VECTOR('',#4428,1.);
#1324=VECTOR('',#4429,1.);
#1325=VECTOR('',#4432,1.);
#1326=VECTOR('',#4433,1.);
#1327=VECTOR('',#4434,1.);
#1328=VECTOR('',#4437,1.);
#1329=VECTOR('',#4438,1.);
#1330=VECTOR('',#4453,0.325);
#1331=VECTOR('',#4458,0.35);
#1332=VECTOR('',#4463,0.335);
#1333=VECTOR('',#4472,0.21);
#1334=VECTOR('',#4477,0.2);
#1335=VECTOR('',#4482,0.18);
#1336=VECTOR('',#4487,1.);
#1337=VECTOR('',#4488,1.);
#1338=VECTOR('',#4489,1.);
#1339=VECTOR('',#4490,1.);
#1340=VECTOR('',#4493,1.);
#1341=VECTOR('',#4494,1.);
#1342=VECTOR('',#4495,1.);
#1343=VECTOR('',#4498,1.);
#1344=VECTOR('',#4499,1.);
#1345=VECTOR('',#4500,1.);
#1346=VECTOR('',#4503,1.);
#1347=VECTOR('',#4504,1.);
#1348=VECTOR('',#4505,1.);
#1349=VECTOR('',#4508,1.);
#1350=VECTOR('',#4509,1.);
#1351=VECTOR('',#4510,1.);
#1352=VECTOR('',#4513,1.);
#1353=VECTOR('',#4514,1.);
#1354=VECTOR('',#4525,0.42);
#1355=VECTOR('',#4532,0.8);
#1356=VECTOR('',#4563,0.734027674973257);
#1357=VECTOR('',#4570,0.734027674973257);
#1358=VECTOR('',#4573,1.);
#1359=VECTOR('',#4574,1.);
#1360=VECTOR('',#4577,1.);
#1361=VECTOR('',#4580,1.);
#1362=VECTOR('',#4585,0.4);
#1363=VECTOR('',#4590,1.);
#1364=VECTOR('',#4593,1.);
#1365=VECTOR('',#4604,1.);
#1366=VECTOR('',#4607,1.);
#1367=VECTOR('',#4612,1.);
#1368=VECTOR('',#4615,1.);
#1369=VECTOR('',#4620,1.);
#1370=VECTOR('',#4623,1.);
#1371=VECTOR('',#4628,1.);
#1372=VECTOR('',#4631,1.);
#1373=VECTOR('',#4636,1.);
#1374=VECTOR('',#4639,1.);
#1375=VECTOR('',#4644,1.);
#1376=VECTOR('',#4647,1.);
#1377=VECTOR('',#4692,1.);
#1378=VECTOR('',#4693,1.);
#1379=VECTOR('',#4694,1.);
#1380=VECTOR('',#4695,1.);
#1381=VECTOR('',#4698,1.);
#1382=VECTOR('',#4699,1.);
#1383=VECTOR('',#4700,1.);
#1384=VECTOR('',#4703,1.);
#1385=VECTOR('',#4704,1.);
#1386=VECTOR('',#4705,1.);
#1387=VECTOR('',#4708,1.);
#1388=VECTOR('',#4709,1.);
#1389=VECTOR('',#4710,1.);
#1390=VECTOR('',#4713,1.);
#1391=VECTOR('',#4714,1.);
#1392=VECTOR('',#4715,1.);
#1393=VECTOR('',#4718,1.);
#1394=VECTOR('',#4719,1.);
#1395=VECTOR('',#4726,0.425);
#1396=CIRCLE('',#3472,0.800000000000001);
#1397=CIRCLE('',#3473,0.800000000000001);
#1398=CIRCLE('',#3475,0.275);
#1399=CIRCLE('',#3477,0.8);
#1400=CIRCLE('',#3478,0.8);
#1401=CIRCLE('',#3480,0.275);
#1402=CIRCLE('',#3482,0.275);
#1403=CIRCLE('',#3484,0.275);
#1404=CIRCLE('',#3486,0.425);
#1405=CIRCLE('',#3487,0.425);
#1406=CIRCLE('',#3489,1.3);
#1407=CIRCLE('',#3490,1.3);
#1408=CIRCLE('',#3502,0.2117);
#1409=CIRCLE('',#3511,0.2117);
#1410=CIRCLE('',#3512,0.2117);
#1411=CIRCLE('',#3514,0.2117);
#1412=CIRCLE('',#3521,0.285);
#1413=CIRCLE('',#3522,0.265);
#1414=CIRCLE('',#3524,0.265);
#1415=CIRCLE('',#3526,0.5);
#1416=CIRCLE('',#3528,0.5);
#1417=CIRCLE('',#3532,0.25);
#1418=CIRCLE('',#3533,0.24505);
#1419=CIRCLE('',#3535,0.25);
#1420=CIRCLE('',#3538,0.375);
#1421=CIRCLE('',#3540,0.425);
#1422=CIRCLE('',#3542,0.425);
#1423=CIRCLE('',#3544,0.395);
#1424=CIRCLE('',#3546,0.27);
#1425=CIRCLE('',#3548,0.24505);
#1426=CIRCLE('',#3596,0.21);
#1427=CIRCLE('',#3597,0.21);
#1428=CIRCLE('',#3610,0.3933);
#1429=CIRCLE('',#3611,0.3933);
#1430=CIRCLE('',#3613,0.32);
#1431=CIRCLE('',#3616,0.6175);
#1432=CIRCLE('',#3628,0.164999999999999);
#1433=CIRCLE('',#3629,0.164999999999999);
#1434=CIRCLE('',#3631,0.164999999999999);
#1435=CIRCLE('',#3632,0.164999999999999);
#1436=CIRCLE('',#3634,1.8);
#1437=CIRCLE('',#3635,1.8);
#1438=CIRCLE('',#3636,0.425);
#1439=CIRCLE('',#3641,1.8);
#1440=CIRCLE('',#3643,1.8);
#1441=CIRCLE('',#3645,0.425);
#1442=CIRCLE('',#3649,0.4);
#1443=CIRCLE('',#3650,0.4);
#1444=CIRCLE('',#3652,0.225);
#1445=CIRCLE('',#3654,0.4);
#1446=CIRCLE('',#3655,0.4);
#1447=CIRCLE('',#3657,0.225);
#1448=CIRCLE('',#3659,0.225);
#1449=CIRCLE('',#3661,0.225);
#1450=CIRCLE('',#3670,0.3);
#1451=CIRCLE('',#3672,0.35);
#1452=CIRCLE('',#3674,0.35);
#1453=CIRCLE('',#3676,0.32);
#1454=CIRCLE('',#3678,0.22);
#1455=CIRCLE('',#3680,0.1954);
#1456=CIRCLE('',#3682,0.1954);
#1457=CIRCLE('',#3684,0.16);
#1458=CIRCLE('',#3696,0.42);
#1459=CIRCLE('',#3697,0.42);
#1460=CIRCLE('',#3699,0.8);
#1461=CIRCLE('',#3700,0.8);
#1462=CIRCLE('',#3715,0.6175);
#1463=CIRCLE('',#3717,0.6175);
#1464=CIRCLE('',#3722,0.338975);
#1465=CIRCLE('',#3723,0.338975);
#1466=CIRCLE('',#3731,0.4);
#1467=CIRCLE('',#3732,0.4);
#1468=CIRCLE('',#3734,0.4);
#1469=CIRCLE('',#3735,0.4);
#1470=CIRCLE('',#3737,0.4);
#1471=CIRCLE('',#3738,0.4);
#1472=CIRCLE('',#3740,0.4);
#1473=CIRCLE('',#3741,0.4);
#1474=CIRCLE('',#3743,0.4);
#1475=CIRCLE('',#3744,0.4);
#1476=CIRCLE('',#3746,0.4);
#1477=CIRCLE('',#3747,0.4);
#1478=CIRCLE('',#3749,1.8);
#1479=CIRCLE('',#3750,1.8);
#1480=CIRCLE('',#3751,1.8);
#1481=CIRCLE('',#3752,1.8);
#1482=CIRCLE('',#3753,1.8);
#1483=CIRCLE('',#3754,1.8);
#1484=CIRCLE('',#3755,0.425);
#1485=CIRCLE('',#3757,1.8);
#1486=CIRCLE('',#3759,1.8);
#1487=CIRCLE('',#3761,1.8);
#1488=CIRCLE('',#3763,1.8);
#1489=CIRCLE('',#3765,1.8);
#1490=CIRCLE('',#3767,1.8);
#1491=CIRCLE('',#3775,0.425);
#1492=VERTEX_POINT('',#4751);
#1493=VERTEX_POINT('',#4753);
#1494=VERTEX_POINT('',#4757);
#1495=VERTEX_POINT('',#4760);
#1496=VERTEX_POINT('',#4762);
#1497=VERTEX_POINT('',#4766);
#1498=VERTEX_POINT('',#4769);
#1499=VERTEX_POINT('',#4773);
#1500=VERTEX_POINT('',#4777);
#1501=VERTEX_POINT('',#4779);
#1502=VERTEX_POINT('',#4783);
#1503=VERTEX_POINT('',#4785);
#1504=VERTEX_POINT('',#4790);
#1505=VERTEX_POINT('',#4791);
#1506=VERTEX_POINT('',#4793);
#1507=VERTEX_POINT('',#4795);
#1508=VERTEX_POINT('',#4799);
#1509=VERTEX_POINT('',#4801);
#1510=VERTEX_POINT('',#4805);
#1511=VERTEX_POINT('',#4807);
#1512=VERTEX_POINT('',#4817);
#1513=VERTEX_POINT('',#4818);
#1514=VERTEX_POINT('',#4820);
#1515=VERTEX_POINT('',#4822);
#1516=VERTEX_POINT('',#4826);
#1517=VERTEX_POINT('',#4828);
#1518=VERTEX_POINT('',#4832);
#1519=VERTEX_POINT('',#4834);
#1520=VERTEX_POINT('',#4837);
#1521=VERTEX_POINT('',#4840);
#1522=VERTEX_POINT('',#4842);
#1523=VERTEX_POINT('',#4844);
#1524=VERTEX_POINT('',#4846);
#1525=VERTEX_POINT('',#4848);
#1526=VERTEX_POINT('',#4850);
#1527=VERTEX_POINT('',#4854);
#1528=VERTEX_POINT('',#4858);
#1529=VERTEX_POINT('',#4862);
#1530=VERTEX_POINT('',#4864);
#1531=VERTEX_POINT('',#4866);
#1532=VERTEX_POINT('',#4868);
#1533=VERTEX_POINT('',#4874);
#1534=VERTEX_POINT('',#4876);
#1535=VERTEX_POINT('',#4880);
#1536=VERTEX_POINT('',#4883);
#1537=VERTEX_POINT('',#4885);
#1538=VERTEX_POINT('',#4897);
#1539=VERTEX_POINT('',#4899);
#1540=VERTEX_POINT('',#4903);
#1541=VERTEX_POINT('',#4907);
#1542=VERTEX_POINT('',#4910);
#1543=VERTEX_POINT('',#4916);
#1544=VERTEX_POINT('',#4918);
#1545=VERTEX_POINT('',#4921);
#1546=VERTEX_POINT('',#4926);
#1547=VERTEX_POINT('',#4929);
#1548=VERTEX_POINT('',#4933);
#1549=VERTEX_POINT('',#4937);
#1550=VERTEX_POINT('',#4941);
#1551=VERTEX_POINT('',#4944);
#1552=VERTEX_POINT('',#4950);
#1553=VERTEX_POINT('',#4951);
#1554=VERTEX_POINT('',#4953);
#1555=VERTEX_POINT('',#4955);
#1556=VERTEX_POINT('',#4959);
#1557=VERTEX_POINT('',#4961);
#1558=VERTEX_POINT('',#4965);
#1559=VERTEX_POINT('',#4967);
#1560=VERTEX_POINT('',#4971);
#1561=VERTEX_POINT('',#4973);
#1562=VERTEX_POINT('',#4977);
#1563=VERTEX_POINT('',#4979);
#1564=VERTEX_POINT('',#4989);
#1565=VERTEX_POINT('',#4990);
#1566=VERTEX_POINT('',#4992);
#1567=VERTEX_POINT('',#4994);
#1568=VERTEX_POINT('',#4998);
#1569=VERTEX_POINT('',#5000);
#1570=VERTEX_POINT('',#5004);
#1571=VERTEX_POINT('',#5006);
#1572=VERTEX_POINT('',#5010);
#1573=VERTEX_POINT('',#5012);
#1574=VERTEX_POINT('',#5016);
#1575=VERTEX_POINT('',#5018);
#1576=VERTEX_POINT('',#5022);
#1577=VERTEX_POINT('',#5024);
#1578=VERTEX_POINT('',#5028);
#1579=VERTEX_POINT('',#5030);
#1580=VERTEX_POINT('',#5034);
#1581=VERTEX_POINT('',#5036);
#1582=VERTEX_POINT('',#5040);
#1583=VERTEX_POINT('',#5042);
#1584=VERTEX_POINT('',#5046);
#1585=VERTEX_POINT('',#5047);
#1586=VERTEX_POINT('',#5049);
#1587=VERTEX_POINT('',#5051);
#1588=VERTEX_POINT('',#5055);
#1589=VERTEX_POINT('',#5057);
#1590=VERTEX_POINT('',#5061);
#1591=VERTEX_POINT('',#5063);
#1592=VERTEX_POINT('',#5067);
#1593=VERTEX_POINT('',#5069);
#1594=VERTEX_POINT('',#5073);
#1595=VERTEX_POINT('',#5075);
#1596=VERTEX_POINT('',#5079);
#1597=VERTEX_POINT('',#5081);
#1598=VERTEX_POINT('',#5085);
#1599=VERTEX_POINT('',#5087);
#1600=VERTEX_POINT('',#5091);
#1601=VERTEX_POINT('',#5093);
#1602=VERTEX_POINT('',#5097);
#1603=VERTEX_POINT('',#5099);
#1604=VERTEX_POINT('',#5103);
#1605=VERTEX_POINT('',#5104);
#1606=VERTEX_POINT('',#5106);
#1607=VERTEX_POINT('',#5108);
#1608=VERTEX_POINT('',#5112);
#1609=VERTEX_POINT('',#5114);
#1610=VERTEX_POINT('',#5118);
#1611=VERTEX_POINT('',#5120);
#1612=VERTEX_POINT('',#5124);
#1613=VERTEX_POINT('',#5126);
#1614=VERTEX_POINT('',#5130);
#1615=VERTEX_POINT('',#5132);
#1616=VERTEX_POINT('',#5136);
#1617=VERTEX_POINT('',#5138);
#1618=VERTEX_POINT('',#5142);
#1619=VERTEX_POINT('',#5144);
#1620=VERTEX_POINT('',#5148);
#1621=VERTEX_POINT('',#5150);
#1622=VERTEX_POINT('',#5154);
#1623=VERTEX_POINT('',#5156);
#1624=VERTEX_POINT('',#5160);
#1625=VERTEX_POINT('',#5161);
#1626=VERTEX_POINT('',#5163);
#1627=VERTEX_POINT('',#5165);
#1628=VERTEX_POINT('',#5169);
#1629=VERTEX_POINT('',#5171);
#1630=VERTEX_POINT('',#5175);
#1631=VERTEX_POINT('',#5177);
#1632=VERTEX_POINT('',#5181);
#1633=VERTEX_POINT('',#5183);
#1634=VERTEX_POINT('',#5187);
#1635=VERTEX_POINT('',#5189);
#1636=VERTEX_POINT('',#5193);
#1637=VERTEX_POINT('',#5195);
#1638=VERTEX_POINT('',#5199);
#1639=VERTEX_POINT('',#5201);
#1640=VERTEX_POINT('',#5205);
#1641=VERTEX_POINT('',#5207);
#1642=VERTEX_POINT('',#5211);
#1643=VERTEX_POINT('',#5213);
#1644=VERTEX_POINT('',#5217);
#1645=VERTEX_POINT('',#5219);
#1646=VERTEX_POINT('',#5223);
#1647=VERTEX_POINT('',#5225);
#1648=VERTEX_POINT('',#5229);
#1649=VERTEX_POINT('',#5231);
#1650=VERTEX_POINT('',#5238);
#1651=VERTEX_POINT('',#5240);
#1652=VERTEX_POINT('',#5247);
#1653=VERTEX_POINT('',#5249);
#1654=VERTEX_POINT('',#5262);
#1655=VERTEX_POINT('',#5264);
#1656=VERTEX_POINT('',#5268);
#1657=VERTEX_POINT('',#5273);
#1658=VERTEX_POINT('',#5275);
#1659=VERTEX_POINT('',#5277);
#1660=VERTEX_POINT('',#5281);
#1661=VERTEX_POINT('',#5285);
#1662=VERTEX_POINT('',#5289);
#1663=VERTEX_POINT('',#5293);
#1664=VERTEX_POINT('',#5301);
#1665=VERTEX_POINT('',#5303);
#1666=VERTEX_POINT('',#5307);
#1667=VERTEX_POINT('',#5311);
#1668=VERTEX_POINT('',#5315);
#1669=VERTEX_POINT('',#5319);
#1670=VERTEX_POINT('',#5329);
#1671=VERTEX_POINT('',#5331);
#1672=VERTEX_POINT('',#5335);
#1673=VERTEX_POINT('',#5337);
#1674=VERTEX_POINT('',#5341);
#1675=VERTEX_POINT('',#5342);
#1676=VERTEX_POINT('',#5344);
#1677=VERTEX_POINT('',#5346);
#1678=VERTEX_POINT('',#5348);
#1679=VERTEX_POINT('',#5351);
#1680=VERTEX_POINT('',#5354);
#1681=VERTEX_POINT('',#5356);
#1682=VERTEX_POINT('',#5360);
#1683=VERTEX_POINT('',#5364);
#1684=VERTEX_POINT('',#5370);
#1685=VERTEX_POINT('',#5374);
#1686=VERTEX_POINT('',#5380);
#1687=VERTEX_POINT('',#5382);
#1688=VERTEX_POINT('',#5386);
#1689=VERTEX_POINT('',#5389);
#1690=VERTEX_POINT('',#5391);
#1691=VERTEX_POINT('',#5395);
#1692=VERTEX_POINT('',#5398);
#1693=VERTEX_POINT('',#5402);
#1694=VERTEX_POINT('',#5406);
#1695=VERTEX_POINT('',#5407);
#1696=VERTEX_POINT('',#5409);
#1697=VERTEX_POINT('',#5411);
#1698=VERTEX_POINT('',#5415);
#1699=VERTEX_POINT('',#5417);
#1700=VERTEX_POINT('',#5421);
#1701=VERTEX_POINT('',#5423);
#1702=VERTEX_POINT('',#5433);
#1703=VERTEX_POINT('',#5436);
#1704=VERTEX_POINT('',#5440);
#1705=VERTEX_POINT('',#5444);
#1706=VERTEX_POINT('',#5448);
#1707=VERTEX_POINT('',#5451);
#1708=VERTEX_POINT('',#5455);
#1709=VERTEX_POINT('',#5459);
#1710=VERTEX_POINT('',#5464);
#1711=VERTEX_POINT('',#5465);
#1712=VERTEX_POINT('',#5467);
#1713=VERTEX_POINT('',#5469);
#1714=VERTEX_POINT('',#5473);
#1715=VERTEX_POINT('',#5475);
#1716=VERTEX_POINT('',#5479);
#1717=VERTEX_POINT('',#5481);
#1718=VERTEX_POINT('',#5485);
#1719=VERTEX_POINT('',#5487);
#1720=VERTEX_POINT('',#5491);
#1721=VERTEX_POINT('',#5493);
#1722=VERTEX_POINT('',#5503);
#1723=VERTEX_POINT('',#5505);
#1724=VERTEX_POINT('',#5509);
#1725=VERTEX_POINT('',#5511);
#1726=VERTEX_POINT('',#5528);
#1727=VERTEX_POINT('',#5529);
#1728=VERTEX_POINT('',#5533);
#1729=VERTEX_POINT('',#5537);
#1730=VERTEX_POINT('',#5540);
#1731=VERTEX_POINT('',#5544);
#1732=VERTEX_POINT('',#5548);
#1733=VERTEX_POINT('',#5556);
#1734=VERTEX_POINT('',#5558);
#1735=VERTEX_POINT('',#5560);
#1736=VERTEX_POINT('',#5564);
#1737=VERTEX_POINT('',#5568);
#1738=VERTEX_POINT('',#5572);
#1739=VERTEX_POINT('',#5576);
#1740=VERTEX_POINT('',#5591);
#1741=VERTEX_POINT('',#5593);
#1742=VERTEX_POINT('',#5605);
#1743=VERTEX_POINT('',#5606);
#1744=VERTEX_POINT('',#5608);
#1745=VERTEX_POINT('',#5610);
#1746=VERTEX_POINT('',#5614);
#1747=VERTEX_POINT('',#5615);
#1748=VERTEX_POINT('',#5617);
#1749=VERTEX_POINT('',#5619);
#1750=VERTEX_POINT('',#5623);
#1751=VERTEX_POINT('',#5624);
#1752=VERTEX_POINT('',#5626);
#1753=VERTEX_POINT('',#5628);
#1754=VERTEX_POINT('',#5632);
#1755=VERTEX_POINT('',#5633);
#1756=VERTEX_POINT('',#5635);
#1757=VERTEX_POINT('',#5637);
#1758=VERTEX_POINT('',#5641);
#1759=VERTEX_POINT('',#5642);
#1760=VERTEX_POINT('',#5644);
#1761=VERTEX_POINT('',#5646);
#1762=VERTEX_POINT('',#5650);
#1763=VERTEX_POINT('',#5651);
#1764=VERTEX_POINT('',#5653);
#1765=VERTEX_POINT('',#5655);
#1766=VERTEX_POINT('',#5665);
#1767=VERTEX_POINT('',#5680);
#1768=VERTEX_POINT('',#5681);
#1769=VERTEX_POINT('',#5683);
#1770=VERTEX_POINT('',#5685);
#1771=VERTEX_POINT('',#5689);
#1772=VERTEX_POINT('',#5691);
#1773=VERTEX_POINT('',#5695);
#1774=VERTEX_POINT('',#5697);
#1775=VERTEX_POINT('',#5701);
#1776=VERTEX_POINT('',#5703);
#1777=VERTEX_POINT('',#5707);
#1778=VERTEX_POINT('',#5709);
#1779=VERTEX_POINT('',#5716);
#1780=EDGE_CURVE('',#1492,#1492,#1396,.T.);
#1781=EDGE_CURVE('',#1492,#1493,#752,.T.);
#1782=EDGE_CURVE('',#1493,#1493,#1397,.T.);
#1783=EDGE_CURVE('',#1494,#1494,#1398,.T.);
#1784=EDGE_CURVE('',#1495,#1495,#1399,.T.);
#1785=EDGE_CURVE('',#1495,#1496,#753,.T.);
#1786=EDGE_CURVE('',#1496,#1496,#1400,.T.);
#1787=EDGE_CURVE('',#1497,#1497,#1401,.T.);
#1788=EDGE_CURVE('',#1497,#1498,#754,.T.);
#1789=EDGE_CURVE('',#1498,#1498,#1402,.T.);
#1790=EDGE_CURVE('',#1494,#1499,#755,.T.);
#1791=EDGE_CURVE('',#1499,#1499,#1403,.T.);
#1792=EDGE_CURVE('',#1500,#1500,#1404,.T.);
#1793=EDGE_CURVE('',#1500,#1501,#756,.T.);
#1794=EDGE_CURVE('',#1501,#1501,#1405,.T.);
#1795=EDGE_CURVE('',#1502,#1502,#1406,.T.);
#1796=EDGE_CURVE('',#1502,#1503,#757,.T.);
#1797=EDGE_CURVE('',#1503,#1503,#1407,.T.);
#1798=EDGE_CURVE('',#1504,#1505,#758,.T.);
#1799=EDGE_CURVE('',#1505,#1506,#759,.T.);
#1800=EDGE_CURVE('',#1507,#1506,#760,.T.);
#1801=EDGE_CURVE('',#1504,#1507,#761,.T.);
#1802=EDGE_CURVE('',#1508,#1504,#762,.T.);
#1803=EDGE_CURVE('',#1509,#1507,#763,.T.);
#1804=EDGE_CURVE('',#1508,#1509,#764,.T.);
#1805=EDGE_CURVE('',#1510,#1508,#765,.T.);
#1806=EDGE_CURVE('',#1511,#1509,#766,.T.);
#1807=EDGE_CURVE('',#1510,#1511,#767,.T.);
#1808=EDGE_CURVE('',#1505,#1510,#768,.T.);
#1809=EDGE_CURVE('',#1506,#1511,#769,.T.);
#1810=EDGE_CURVE('',#1512,#1513,#770,.T.);
#1811=EDGE_CURVE('',#1514,#1512,#771,.T.);
#1812=EDGE_CURVE('',#1515,#1514,#772,.T.);
#1813=EDGE_CURVE('',#1513,#1515,#773,.T.);
#1814=EDGE_CURVE('',#1514,#1516,#774,.T.);
#1815=EDGE_CURVE('',#1517,#1516,#775,.T.);
#1816=EDGE_CURVE('',#1515,#1517,#776,.T.);
#1817=EDGE_CURVE('',#1516,#1518,#777,.T.);
#1818=EDGE_CURVE('',#1518,#1519,#778,.T.);
#1819=EDGE_CURVE('',#1519,#1517,#779,.T.);
#1820=EDGE_CURVE('',#1520,#1520,#1408,.T.);
#1821=EDGE_CURVE('',#1521,#1512,#780,.T.);
#1822=EDGE_CURVE('',#1522,#1521,#781,.T.);
#1823=EDGE_CURVE('',#1522,#1523,#782,.T.);
#1824=EDGE_CURVE('',#1524,#1523,#783,.T.);
#1825=EDGE_CURVE('',#1524,#1525,#784,.T.);
#1826=EDGE_CURVE('',#1525,#1526,#785,.T.);
#1827=EDGE_CURVE('',#1526,#1518,#786,.T.);
#1828=EDGE_CURVE('',#1526,#1527,#787,.T.);
#1829=EDGE_CURVE('',#1527,#1519,#788,.T.);
#1830=EDGE_CURVE('',#1528,#1525,#789,.T.);
#1831=EDGE_CURVE('',#1527,#1528,#790,.T.);
#1832=EDGE_CURVE('',#1529,#1528,#791,.T.);
#1833=EDGE_CURVE('',#1530,#1529,#792,.T.);
#1834=EDGE_CURVE('',#1530,#1531,#793,.T.);
#1835=EDGE_CURVE('',#1532,#1531,#794,.T.);
#1836=EDGE_CURVE('',#1532,#1513,#795,.T.);
#1837=EDGE_CURVE('',#1529,#1524,#796,.T.);
#1838=EDGE_CURVE('',#1523,#1533,#797,.T.);
#1839=EDGE_CURVE('',#1533,#1534,#121,.T.);
#1840=EDGE_CURVE('',#1534,#1530,#798,.T.);
#1841=EDGE_CURVE('',#1535,#1533,#1409,.F.);
#1842=EDGE_CURVE('',#1535,#1520,#799,.T.);
#1843=EDGE_CURVE('',#1536,#1535,#1410,.F.);
#1844=EDGE_CURVE('',#1537,#1536,#122,.T.);
#1845=EDGE_CURVE('',#1534,#1537,#1411,.F.);
#1846=EDGE_CURVE('',#1536,#1522,#800,.T.);
#1847=EDGE_CURVE('',#1531,#1537,#801,.T.);
#1848=EDGE_CURVE('',#1521,#1532,#802,.T.);
#1849=EDGE_CURVE('',#1538,#1538,#1412,.T.);
#1850=EDGE_CURVE('',#1538,#1539,#803,.T.);
#1851=EDGE_CURVE('',#1539,#1539,#1413,.T.);
#1852=EDGE_CURVE('',#1539,#1540,#804,.T.);
#1853=EDGE_CURVE('',#1540,#1540,#1414,.T.);
#1854=EDGE_CURVE('',#1541,#1541,#1415,.T.);
#1855=EDGE_CURVE('',#1541,#1542,#805,.T.);
#1856=EDGE_CURVE('',#1542,#1542,#1416,.T.);
#1857=EDGE_CURVE('',#1543,#1543,#1417,.T.);
#1858=EDGE_CURVE('',#1544,#1544,#1418,.T.);
#1859=EDGE_CURVE('',#1543,#1545,#806,.T.);
#1860=EDGE_CURVE('',#1545,#1545,#1419,.T.);
#1861=EDGE_CURVE('',#1546,#1546,#1420,.T.);
#1862=EDGE_CURVE('',#1547,#1547,#1421,.T.);
#1863=EDGE_CURVE('',#1547,#1546,#807,.T.);
#1864=EDGE_CURVE('',#1548,#1548,#1422,.T.);
#1865=EDGE_CURVE('',#1548,#1547,#808,.T.);
#1866=EDGE_CURVE('',#1549,#1549,#1423,.T.);
#1867=EDGE_CURVE('',#1549,#1548,#809,.T.);
#1868=EDGE_CURVE('',#1550,#1550,#1424,.T.);
#1869=EDGE_CURVE('',#1551,#1551,#1425,.F.);
#1870=EDGE_CURVE('',#1551,#1550,#810,.T.);
#1871=EDGE_CURVE('',#1544,#1551,#811,.T.);
#1872=EDGE_CURVE('',#1552,#1553,#812,.T.);
#1873=EDGE_CURVE('',#1553,#1554,#813,.T.);
#1874=EDGE_CURVE('',#1554,#1555,#814,.T.);
#1875=EDGE_CURVE('',#1552,#1555,#815,.T.);
#1876=EDGE_CURVE('',#1553,#1556,#816,.T.);
#1877=EDGE_CURVE('',#1556,#1557,#817,.T.);
#1878=EDGE_CURVE('',#1557,#1554,#818,.T.);
#1879=EDGE_CURVE('',#1556,#1558,#819,.T.);
#1880=EDGE_CURVE('',#1558,#1559,#820,.T.);
#1881=EDGE_CURVE('',#1559,#1557,#821,.T.);
#1882=EDGE_CURVE('',#1558,#1560,#822,.T.);
#1883=EDGE_CURVE('',#1560,#1561,#823,.T.);
#1884=EDGE_CURVE('',#1561,#1559,#824,.T.);
#1885=EDGE_CURVE('',#1560,#1562,#825,.T.);
#1886=EDGE_CURVE('',#1562,#1563,#826,.T.);
#1887=EDGE_CURVE('',#1563,#1561,#827,.T.);
#1888=EDGE_CURVE('',#1562,#1552,#828,.T.);
#1889=EDGE_CURVE('',#1555,#1563,#829,.T.);
#1890=EDGE_CURVE('',#1564,#1565,#830,.T.);
#1891=EDGE_CURVE('',#1564,#1566,#831,.T.);
#1892=EDGE_CURVE('',#1567,#1566,#832,.T.);
#1893=EDGE_CURVE('',#1565,#1567,#833,.T.);
#1894=EDGE_CURVE('',#1568,#1564,#834,.T.);
#1895=EDGE_CURVE('',#1568,#1569,#835,.T.);
#1896=EDGE_CURVE('',#1566,#1569,#836,.T.);
#1897=EDGE_CURVE('',#1570,#1568,#837,.T.);
#1898=EDGE_CURVE('',#1570,#1571,#838,.T.);
#1899=EDGE_CURVE('',#1569,#1571,#839,.T.);
#1900=EDGE_CURVE('',#1572,#1570,#840,.T.);
#1901=EDGE_CURVE('',#1572,#1573,#841,.T.);
#1902=EDGE_CURVE('',#1571,#1573,#842,.T.);
#1903=EDGE_CURVE('',#1574,#1572,#843,.T.);
#1904=EDGE_CURVE('',#1574,#1575,#844,.T.);
#1905=EDGE_CURVE('',#1573,#1575,#845,.T.);
#1906=EDGE_CURVE('',#1576,#1574,#846,.T.);
#1907=EDGE_CURVE('',#1576,#1577,#847,.T.);
#1908=EDGE_CURVE('',#1575,#1577,#848,.T.);
#1909=EDGE_CURVE('',#1578,#1576,#849,.T.);
#1910=EDGE_CURVE('',#1578,#1579,#850,.T.);
#1911=EDGE_CURVE('',#1577,#1579,#851,.T.);
#1912=EDGE_CURVE('',#1580,#1578,#852,.T.);
#1913=EDGE_CURVE('',#1580,#1581,#853,.T.);
#1914=EDGE_CURVE('',#1579,#1581,#854,.T.);
#1915=EDGE_CURVE('',#1582,#1580,#855,.T.);
#1916=EDGE_CURVE('',#1583,#1582,#856,.T.);
#1917=EDGE_CURVE('',#1581,#1583,#857,.T.);
#1918=EDGE_CURVE('',#1584,#1585,#858,.T.);
#1919=EDGE_CURVE('',#1584,#1586,#859,.T.);
#1920=EDGE_CURVE('',#1587,#1586,#860,.T.);
#1921=EDGE_CURVE('',#1585,#1587,#861,.T.);
#1922=EDGE_CURVE('',#1588,#1584,#862,.T.);
#1923=EDGE_CURVE('',#1588,#1589,#863,.T.);
#1924=EDGE_CURVE('',#1586,#1589,#864,.T.);
#1925=EDGE_CURVE('',#1590,#1588,#865,.T.);
#1926=EDGE_CURVE('',#1590,#1591,#866,.T.);
#1927=EDGE_CURVE('',#1589,#1591,#867,.T.);
#1928=EDGE_CURVE('',#1592,#1590,#868,.T.);
#1929=EDGE_CURVE('',#1592,#1593,#869,.T.);
#1930=EDGE_CURVE('',#1591,#1593,#870,.T.);
#1931=EDGE_CURVE('',#1594,#1592,#871,.T.);
#1932=EDGE_CURVE('',#1594,#1595,#872,.T.);
#1933=EDGE_CURVE('',#1593,#1595,#873,.T.);
#1934=EDGE_CURVE('',#1596,#1594,#874,.T.);
#1935=EDGE_CURVE('',#1596,#1597,#875,.T.);
#1936=EDGE_CURVE('',#1595,#1597,#876,.T.);
#1937=EDGE_CURVE('',#1598,#1596,#877,.T.);
#1938=EDGE_CURVE('',#1598,#1599,#878,.T.);
#1939=EDGE_CURVE('',#1597,#1599,#879,.T.);
#1940=EDGE_CURVE('',#1600,#1598,#880,.T.);
#1941=EDGE_CURVE('',#1600,#1601,#881,.T.);
#1942=EDGE_CURVE('',#1599,#1601,#882,.T.);
#1943=EDGE_CURVE('',#1602,#1600,#883,.T.);
#1944=EDGE_CURVE('',#1603,#1602,#884,.T.);
#1945=EDGE_CURVE('',#1601,#1603,#885,.T.);
#1946=EDGE_CURVE('',#1604,#1605,#886,.T.);
#1947=EDGE_CURVE('',#1604,#1606,#887,.T.);
#1948=EDGE_CURVE('',#1607,#1606,#888,.T.);
#1949=EDGE_CURVE('',#1605,#1607,#889,.T.);
#1950=EDGE_CURVE('',#1608,#1604,#890,.T.);
#1951=EDGE_CURVE('',#1608,#1609,#891,.T.);
#1952=EDGE_CURVE('',#1606,#1609,#892,.T.);
#1953=EDGE_CURVE('',#1610,#1608,#893,.T.);
#1954=EDGE_CURVE('',#1610,#1611,#894,.T.);
#1955=EDGE_CURVE('',#1609,#1611,#895,.T.);
#1956=EDGE_CURVE('',#1612,#1610,#896,.T.);
#1957=EDGE_CURVE('',#1612,#1613,#897,.T.);
#1958=EDGE_CURVE('',#1611,#1613,#898,.T.);
#1959=EDGE_CURVE('',#1614,#1612,#899,.T.);
#1960=EDGE_CURVE('',#1614,#1615,#900,.T.);
#1961=EDGE_CURVE('',#1613,#1615,#901,.T.);
#1962=EDGE_CURVE('',#1616,#1614,#902,.T.);
#1963=EDGE_CURVE('',#1616,#1617,#903,.T.);
#1964=EDGE_CURVE('',#1615,#1617,#904,.T.);
#1965=EDGE_CURVE('',#1618,#1616,#905,.T.);
#1966=EDGE_CURVE('',#1618,#1619,#906,.T.);
#1967=EDGE_CURVE('',#1617,#1619,#907,.T.);
#1968=EDGE_CURVE('',#1620,#1618,#908,.T.);
#1969=EDGE_CURVE('',#1620,#1621,#909,.T.);
#1970=EDGE_CURVE('',#1619,#1621,#910,.T.);
#1971=EDGE_CURVE('',#1622,#1620,#911,.T.);
#1972=EDGE_CURVE('',#1623,#1622,#912,.T.);
#1973=EDGE_CURVE('',#1621,#1623,#913,.T.);
#1974=EDGE_CURVE('',#1624,#1625,#914,.T.);
#1975=EDGE_CURVE('',#1624,#1626,#915,.T.);
#1976=EDGE_CURVE('',#1627,#1626,#916,.T.);
#1977=EDGE_CURVE('',#1625,#1627,#917,.T.);
#1978=EDGE_CURVE('',#1628,#1624,#918,.T.);
#1979=EDGE_CURVE('',#1628,#1629,#919,.T.);
#1980=EDGE_CURVE('',#1626,#1629,#920,.T.);
#1981=EDGE_CURVE('',#1630,#1628,#921,.T.);
#1982=EDGE_CURVE('',#1630,#1631,#922,.T.);
#1983=EDGE_CURVE('',#1629,#1631,#923,.T.);
#1984=EDGE_CURVE('',#1632,#1630,#924,.T.);
#1985=EDGE_CURVE('',#1632,#1633,#925,.T.);
#1986=EDGE_CURVE('',#1631,#1633,#926,.T.);
#1987=EDGE_CURVE('',#1634,#1632,#927,.T.);
#1988=EDGE_CURVE('',#1634,#1635,#928,.T.);
#1989=EDGE_CURVE('',#1633,#1635,#929,.T.);
#1990=EDGE_CURVE('',#1636,#1634,#930,.T.);
#1991=EDGE_CURVE('',#1636,#1637,#931,.T.);
#1992=EDGE_CURVE('',#1635,#1637,#932,.T.);
#1993=EDGE_CURVE('',#1638,#1636,#933,.T.);
#1994=EDGE_CURVE('',#1638,#1639,#934,.T.);
#1995=EDGE_CURVE('',#1637,#1639,#935,.T.);
#1996=EDGE_CURVE('',#1640,#1638,#936,.T.);
#1997=EDGE_CURVE('',#1640,#1641,#937,.T.);
#1998=EDGE_CURVE('',#1639,#1641,#938,.T.);
#1999=EDGE_CURVE('',#1642,#1640,#939,.T.);
#2000=EDGE_CURVE('',#1643,#1642,#940,.T.);
#2001=EDGE_CURVE('',#1641,#1643,#941,.T.);
#2002=EDGE_CURVE('',#1644,#1644,#1426,.T.);
#2003=EDGE_CURVE('',#1644,#1645,#942,.T.);
#2004=EDGE_CURVE('',#1645,#1645,#1427,.T.);
#2005=EDGE_CURVE('',#1582,#1646,#943,.T.);
#2006=EDGE_CURVE('',#1646,#1647,#944,.T.);
#2007=EDGE_CURVE('',#1583,#1647,#945,.T.);
#2008=EDGE_CURVE('',#1648,#1567,#946,.T.);
#2009=EDGE_CURVE('',#1649,#1648,#947,.T.);
#2010=EDGE_CURVE('',#1649,#1565,#948,.T.);
#2011=EDGE_CURVE('',#1602,#1649,#949,.T.);
#2012=EDGE_CURVE('',#1603,#1648,#950,.T.);
#2013=EDGE_CURVE('',#1650,#1587,#951,.T.);
#2014=EDGE_CURVE('',#1651,#1650,#952,.T.);
#2015=EDGE_CURVE('',#1651,#1585,#953,.T.);
#2016=EDGE_CURVE('',#1622,#1651,#954,.T.);
#2017=EDGE_CURVE('',#1623,#1650,#955,.T.);
#2018=EDGE_CURVE('',#1652,#1607,#956,.T.);
#2019=EDGE_CURVE('',#1653,#1652,#957,.T.);
#2020=EDGE_CURVE('',#1653,#1605,#958,.T.);
#2021=EDGE_CURVE('',#1642,#1653,#959,.T.);
#2022=EDGE_CURVE('',#1643,#1652,#960,.T.);
#2023=EDGE_CURVE('',#1647,#1627,#961,.T.);
#2024=EDGE_CURVE('',#1646,#1625,#962,.T.);
#2025=EDGE_CURVE('',#1654,#1654,#1428,.F.);
#2026=EDGE_CURVE('',#1654,#1655,#963,.T.);
#2027=EDGE_CURVE('',#1655,#1655,#1429,.F.);
#2028=EDGE_CURVE('',#1656,#1656,#1430,.T.);
#2029=EDGE_CURVE('',#1656,#1654,#964,.T.);
#2030=EDGE_CURVE('',#1657,#1657,#1431,.T.);
#2031=EDGE_CURVE('',#1657,#1658,#965,.T.);
#2032=EDGE_CURVE('',#1659,#1658,#87,.T.);
#2033=EDGE_CURVE('',#1660,#1659,#88,.T.);
#2034=EDGE_CURVE('',#1661,#1660,#89,.T.);
#2035=EDGE_CURVE('',#1662,#1661,#90,.T.);
#2036=EDGE_CURVE('',#1663,#1662,#91,.T.);
#2037=EDGE_CURVE('',#1658,#1663,#92,.T.);
#2038=EDGE_CURVE('',#1664,#1662,#966,.T.);
#2039=EDGE_CURVE('',#1664,#1665,#967,.T.);
#2040=EDGE_CURVE('',#1665,#1663,#968,.T.);
#2041=EDGE_CURVE('',#1666,#1661,#969,.T.);
#2042=EDGE_CURVE('',#1666,#1664,#970,.T.);
#2043=EDGE_CURVE('',#1667,#1660,#971,.T.);
#2044=EDGE_CURVE('',#1667,#1666,#972,.T.);
#2045=EDGE_CURVE('',#1668,#1659,#973,.T.);
#2046=EDGE_CURVE('',#1668,#1667,#974,.T.);
#2047=EDGE_CURVE('',#1669,#1658,#975,.T.);
#2048=EDGE_CURVE('',#1669,#1668,#976,.T.);
#2049=EDGE_CURVE('',#1665,#1669,#977,.T.);
#2050=EDGE_CURVE('',#1670,#1670,#1432,.T.);
#2051=EDGE_CURVE('',#1670,#1671,#978,.T.);
#2052=EDGE_CURVE('',#1671,#1671,#1433,.T.);
#2053=EDGE_CURVE('',#1672,#1672,#1434,.T.);
#2054=EDGE_CURVE('',#1672,#1673,#979,.T.);
#2055=EDGE_CURVE('',#1673,#1673,#1435,.T.);
#2056=EDGE_CURVE('',#1674,#1675,#1436,.T.);
#2057=EDGE_CURVE('',#1675,#1676,#1437,.T.);
#2058=EDGE_CURVE('',#1676,#1677,#980,.T.);
#2059=EDGE_CURVE('',#1677,#1678,#981,.T.);
#2060=EDGE_CURVE('',#1678,#1674,#982,.T.);
#2061=EDGE_CURVE('',#1679,#1679,#1438,.T.);
#2062=EDGE_CURVE('',#1674,#1680,#983,.T.);
#2063=EDGE_CURVE('',#1681,#1678,#984,.T.);
#2064=EDGE_CURVE('',#1681,#1680,#985,.T.);
#2065=EDGE_CURVE('',#1682,#1681,#986,.T.);
#2066=EDGE_CURVE('',#1682,#1677,#987,.T.);
#2067=EDGE_CURVE('',#1683,#1676,#988,.T.);
#2068=EDGE_CURVE('',#1683,#1682,#989,.T.);
#2069=EDGE_CURVE('',#1680,#1683,#1439,.T.);
#2070=EDGE_CURVE('',#1675,#1684,#990,.T.);
#2071=EDGE_CURVE('',#1684,#1684,#1440,.T.);
#2072=EDGE_CURVE('',#1679,#1685,#991,.T.);
#2073=EDGE_CURVE('',#1685,#1685,#1441,.T.);
#2074=EDGE_CURVE('',#1686,#1686,#1442,.T.);
#2075=EDGE_CURVE('',#1686,#1687,#992,.T.);
#2076=EDGE_CURVE('',#1687,#1687,#1443,.T.);
#2077=EDGE_CURVE('',#1688,#1688,#1444,.T.);
#2078=EDGE_CURVE('',#1689,#1689,#1445,.T.);
#2079=EDGE_CURVE('',#1689,#1690,#993,.T.);
#2080=EDGE_CURVE('',#1690,#1690,#1446,.T.);
#2081=EDGE_CURVE('',#1691,#1691,#1447,.T.);
#2082=EDGE_CURVE('',#1692,#1692,#1448,.T.);
#2083=EDGE_CURVE('',#1692,#1688,#994,.T.);
#2084=EDGE_CURVE('',#1693,#1693,#1449,.T.);
#2085=EDGE_CURVE('',#1693,#1691,#995,.T.);
#2086=EDGE_CURVE('',#1694,#1695,#996,.T.);
#2087=EDGE_CURVE('',#1695,#1696,#997,.T.);
#2088=EDGE_CURVE('',#1697,#1696,#998,.T.);
#2089=EDGE_CURVE('',#1694,#1697,#999,.T.);
#2090=EDGE_CURVE('',#1698,#1694,#1000,.T.);
#2091=EDGE_CURVE('',#1699,#1697,#1001,.T.);
#2092=EDGE_CURVE('',#1698,#1699,#1002,.T.);
#2093=EDGE_CURVE('',#1700,#1698,#1003,.T.);
#2094=EDGE_CURVE('',#1701,#1699,#1004,.T.);
#2095=EDGE_CURVE('',#1700,#1701,#1005,.T.);
#2096=EDGE_CURVE('',#1695,#1700,#1006,.T.);
#2097=EDGE_CURVE('',#1696,#1701,#1007,.T.);
#2098=EDGE_CURVE('',#1702,#1702,#1450,.T.);
#2099=EDGE_CURVE('',#1703,#1703,#1451,.T.);
#2100=EDGE_CURVE('',#1703,#1702,#1008,.T.);
#2101=EDGE_CURVE('',#1704,#1704,#1452,.T.);
#2102=EDGE_CURVE('',#1704,#1703,#1009,.T.);
#2103=EDGE_CURVE('',#1705,#1705,#1453,.T.);
#2104=EDGE_CURVE('',#1705,#1704,#1010,.T.);
#2105=EDGE_CURVE('',#1706,#1706,#1454,.T.);
#2106=EDGE_CURVE('',#1707,#1707,#1455,.F.);
#2107=EDGE_CURVE('',#1707,#1706,#1011,.T.);
#2108=EDGE_CURVE('',#1708,#1708,#1456,.F.);
#2109=EDGE_CURVE('',#1708,#1707,#1012,.T.);
#2110=EDGE_CURVE('',#1709,#1709,#1457,.T.);
#2111=EDGE_CURVE('',#1709,#1708,#1013,.T.);
#2112=EDGE_CURVE('',#1710,#1711,#1014,.T.);
#2113=EDGE_CURVE('',#1711,#1712,#1015,.T.);
#2114=EDGE_CURVE('',#1712,#1713,#1016,.T.);
#2115=EDGE_CURVE('',#1710,#1713,#1017,.T.);
#2116=EDGE_CURVE('',#1711,#1714,#1018,.T.);
#2117=EDGE_CURVE('',#1714,#1715,#1019,.T.);
#2118=EDGE_CURVE('',#1715,#1712,#1020,.T.);
#2119=EDGE_CURVE('',#1714,#1716,#1021,.T.);
#2120=EDGE_CURVE('',#1716,#1717,#1022,.T.);
#2121=EDGE_CURVE('',#1717,#1715,#1023,.T.);
#2122=EDGE_CURVE('',#1716,#1718,#1024,.T.);
#2123=EDGE_CURVE('',#1718,#1719,#1025,.T.);
#2124=EDGE_CURVE('',#1719,#1717,#1026,.T.);
#2125=EDGE_CURVE('',#1718,#1720,#1027,.T.);
#2126=EDGE_CURVE('',#1720,#1721,#1028,.T.);
#2127=EDGE_CURVE('',#1721,#1719,#1029,.T.);
#2128=EDGE_CURVE('',#1720,#1710,#1030,.T.);
#2129=EDGE_CURVE('',#1713,#1721,#1031,.T.);
#2130=EDGE_CURVE('',#1722,#1722,#1458,.T.);
#2131=EDGE_CURVE('',#1722,#1723,#1032,.T.);
#2132=EDGE_CURVE('',#1723,#1723,#1459,.T.);
#2133=EDGE_CURVE('',#1724,#1724,#1460,.T.);
#2134=EDGE_CURVE('',#1724,#1725,#1033,.T.);
#2135=EDGE_CURVE('',#1725,#1725,#1461,.T.);
#2136=EDGE_CURVE('',#1726,#1727,#93,.T.);
#2137=EDGE_CURVE('',#1728,#1726,#94,.T.);
#2138=EDGE_CURVE('',#1728,#1729,#1034,.T.);
#2139=EDGE_CURVE('',#1729,#1729,#1462,.T.);
#2140=EDGE_CURVE('',#1730,#1728,#95,.T.);
#2141=EDGE_CURVE('',#1731,#1730,#96,.T.);
#2142=EDGE_CURVE('',#1732,#1731,#97,.T.);
#2143=EDGE_CURVE('',#1727,#1732,#98,.T.);
#2144=EDGE_CURVE('',#1733,#1733,#1463,.T.);
#2145=EDGE_CURVE('',#1733,#1734,#1035,.T.);
#2146=EDGE_CURVE('',#1735,#1734,#99,.T.);
#2147=EDGE_CURVE('',#1736,#1735,#100,.T.);
#2148=EDGE_CURVE('',#1737,#1736,#101,.T.);
#2149=EDGE_CURVE('',#1738,#1737,#102,.T.);
#2150=EDGE_CURVE('',#1739,#1738,#103,.T.);
#2151=EDGE_CURVE('',#1734,#1739,#104,.T.);
#2152=EDGE_CURVE('',#1730,#1739,#1036,.T.);
#2153=EDGE_CURVE('',#1731,#1738,#1037,.T.);
#2154=EDGE_CURVE('',#1728,#1734,#1038,.T.);
#2155=EDGE_CURVE('',#1726,#1735,#1039,.T.);
#2156=EDGE_CURVE('',#1740,#1740,#1464,.F.);
#2157=EDGE_CURVE('',#1740,#1741,#1040,.T.);
#2158=EDGE_CURVE('',#1741,#1741,#1465,.F.);
#2159=EDGE_CURVE('',#1727,#1736,#1041,.T.);
#2160=EDGE_CURVE('',#1732,#1737,#1042,.T.);
#2161=EDGE_CURVE('',#1742,#1743,#1043,.T.);
#2162=EDGE_CURVE('',#1744,#1742,#1466,.T.);
#2163=EDGE_CURVE('',#1745,#1744,#1044,.T.);
#2164=EDGE_CURVE('',#1743,#1745,#1467,.T.);
#2165=EDGE_CURVE('',#1746,#1747,#1045,.T.);
#2166=EDGE_CURVE('',#1748,#1746,#1468,.T.);
#2167=EDGE_CURVE('',#1749,#1748,#1046,.T.);
#2168=EDGE_CURVE('',#1747,#1749,#1469,.T.);
#2169=EDGE_CURVE('',#1750,#1751,#1047,.T.);
#2170=EDGE_CURVE('',#1752,#1750,#1470,.T.);
#2171=EDGE_CURVE('',#1753,#1752,#1048,.T.);
#2172=EDGE_CURVE('',#1751,#1753,#1471,.T.);
#2173=EDGE_CURVE('',#1754,#1755,#1049,.T.);
#2174=EDGE_CURVE('',#1756,#1754,#1472,.T.);
#2175=EDGE_CURVE('',#1757,#1756,#1050,.T.);
#2176=EDGE_CURVE('',#1755,#1757,#1473,.T.);
#2177=EDGE_CURVE('',#1758,#1759,#1051,.T.);
#2178=EDGE_CURVE('',#1760,#1758,#1474,.T.);
#2179=EDGE_CURVE('',#1761,#1760,#1052,.T.);
#2180=EDGE_CURVE('',#1759,#1761,#1475,.T.);
#2181=EDGE_CURVE('',#1762,#1763,#1053,.T.);
#2182=EDGE_CURVE('',#1764,#1762,#1476,.T.);
#2183=EDGE_CURVE('',#1765,#1764,#1054,.T.);
#2184=EDGE_CURVE('',#1763,#1765,#1477,.T.);
#2185=EDGE_CURVE('',#1742,#1764,#1478,.T.);
#2186=EDGE_CURVE('',#1762,#1747,#1479,.T.);
#2187=EDGE_CURVE('',#1749,#1752,#1480,.T.);
#2188=EDGE_CURVE('',#1750,#1756,#1481,.T.);
#2189=EDGE_CURVE('',#1754,#1760,#1482,.T.);
#2190=EDGE_CURVE('',#1758,#1744,#1483,.T.);
#2191=EDGE_CURVE('',#1766,#1766,#1484,.T.);
#2192=EDGE_CURVE('',#1755,#1761,#1485,.T.);
#2193=EDGE_CURVE('',#1751,#1757,#1486,.T.);
#2194=EDGE_CURVE('',#1763,#1746,#1487,.T.);
#2195=EDGE_CURVE('',#1748,#1753,#1488,.T.);
#2196=EDGE_CURVE('',#1743,#1765,#1489,.T.);
#2197=EDGE_CURVE('',#1759,#1745,#1490,.T.);
#2198=EDGE_CURVE('',#1767,#1768,#1055,.T.);
#2199=EDGE_CURVE('',#1767,#1769,#1056,.T.);
#2200=EDGE_CURVE('',#1769,#1770,#1057,.T.);
#2201=EDGE_CURVE('',#1768,#1770,#1058,.T.);
#2202=EDGE_CURVE('',#1768,#1771,#1059,.T.);
#2203=EDGE_CURVE('',#1770,#1772,#1060,.T.);
#2204=EDGE_CURVE('',#1771,#1772,#1061,.T.);
#2205=EDGE_CURVE('',#1771,#1773,#1062,.T.);
#2206=EDGE_CURVE('',#1772,#1774,#1063,.T.);
#2207=EDGE_CURVE('',#1773,#1774,#1064,.T.);
#2208=EDGE_CURVE('',#1773,#1775,#1065,.T.);
#2209=EDGE_CURVE('',#1774,#1776,#1066,.T.);
#2210=EDGE_CURVE('',#1775,#1776,#1067,.T.);
#2211=EDGE_CURVE('',#1777,#1767,#1068,.T.);
#2212=EDGE_CURVE('',#1777,#1778,#1069,.T.);
#2213=EDGE_CURVE('',#1778,#1769,#1070,.T.);
#2214=EDGE_CURVE('',#1775,#1777,#1071,.T.);
#2215=EDGE_CURVE('',#1776,#1778,#1072,.T.);
#2216=EDGE_CURVE('',#1779,#1779,#1491,.T.);
#2217=EDGE_CURVE('',#1766,#1779,#1073,.T.);
#2218=ORIENTED_EDGE('',*,*,#1780,.F.);
#2219=ORIENTED_EDGE('',*,*,#1781,.T.);
#2220=ORIENTED_EDGE('',*,*,#1782,.T.);
#2221=ORIENTED_EDGE('',*,*,#1781,.F.);
#2222=ORIENTED_EDGE('',*,*,#1782,.F.);
#2223=ORIENTED_EDGE('',*,*,#1783,.F.);
#2224=ORIENTED_EDGE('',*,*,#1784,.F.);
#2225=ORIENTED_EDGE('',*,*,#1785,.T.);
#2226=ORIENTED_EDGE('',*,*,#1786,.T.);
#2227=ORIENTED_EDGE('',*,*,#1785,.F.);
#2228=ORIENTED_EDGE('',*,*,#1786,.F.);
#2229=ORIENTED_EDGE('',*,*,#1787,.F.);
#2230=ORIENTED_EDGE('',*,*,#1787,.T.);
#2231=ORIENTED_EDGE('',*,*,#1788,.T.);
#2232=ORIENTED_EDGE('',*,*,#1789,.F.);
#2233=ORIENTED_EDGE('',*,*,#1788,.F.);
#2234=ORIENTED_EDGE('',*,*,#1783,.T.);
#2235=ORIENTED_EDGE('',*,*,#1790,.T.);
#2236=ORIENTED_EDGE('',*,*,#1791,.F.);
#2237=ORIENTED_EDGE('',*,*,#1790,.F.);
#2238=ORIENTED_EDGE('',*,*,#1792,.F.);
#2239=ORIENTED_EDGE('',*,*,#1793,.T.);
#2240=ORIENTED_EDGE('',*,*,#1794,.F.);
#2241=ORIENTED_EDGE('',*,*,#1793,.F.);
#2242=ORIENTED_EDGE('',*,*,#1795,.F.);
#2243=ORIENTED_EDGE('',*,*,#1796,.T.);
#2244=ORIENTED_EDGE('',*,*,#1797,.F.);
#2245=ORIENTED_EDGE('',*,*,#1796,.F.);
#2246=ORIENTED_EDGE('',*,*,#1795,.T.);
#2247=ORIENTED_EDGE('',*,*,#1794,.T.);
#2248=ORIENTED_EDGE('',*,*,#1798,.T.);
#2249=ORIENTED_EDGE('',*,*,#1799,.T.);
#2250=ORIENTED_EDGE('',*,*,#1800,.F.);
#2251=ORIENTED_EDGE('',*,*,#1801,.F.);
#2252=ORIENTED_EDGE('',*,*,#1802,.T.);
#2253=ORIENTED_EDGE('',*,*,#1801,.T.);
#2254=ORIENTED_EDGE('',*,*,#1803,.F.);
#2255=ORIENTED_EDGE('',*,*,#1804,.F.);
#2256=ORIENTED_EDGE('',*,*,#1805,.T.);
#2257=ORIENTED_EDGE('',*,*,#1804,.T.);
#2258=ORIENTED_EDGE('',*,*,#1806,.F.);
#2259=ORIENTED_EDGE('',*,*,#1807,.F.);
#2260=ORIENTED_EDGE('',*,*,#1808,.T.);
#2261=ORIENTED_EDGE('',*,*,#1807,.T.);
#2262=ORIENTED_EDGE('',*,*,#1809,.F.);
#2263=ORIENTED_EDGE('',*,*,#1799,.F.);
#2264=ORIENTED_EDGE('',*,*,#1809,.T.);
#2265=ORIENTED_EDGE('',*,*,#1806,.T.);
#2266=ORIENTED_EDGE('',*,*,#1803,.T.);
#2267=ORIENTED_EDGE('',*,*,#1800,.T.);
#2268=ORIENTED_EDGE('',*,*,#1789,.T.);
#2269=ORIENTED_EDGE('',*,*,#1791,.T.);
#2270=ORIENTED_EDGE('',*,*,#1797,.T.);
#2271=ORIENTED_EDGE('',*,*,#1808,.F.);
#2272=ORIENTED_EDGE('',*,*,#1798,.F.);
#2273=ORIENTED_EDGE('',*,*,#1802,.F.);
#2274=ORIENTED_EDGE('',*,*,#1805,.F.);
#2275=ORIENTED_EDGE('',*,*,#1780,.T.);
#2276=ORIENTED_EDGE('',*,*,#1784,.T.);
#2277=ORIENTED_EDGE('',*,*,#1792,.T.);
#2278=ORIENTED_EDGE('',*,*,#1810,.F.);
#2279=ORIENTED_EDGE('',*,*,#1811,.F.);
#2280=ORIENTED_EDGE('',*,*,#1812,.F.);
#2281=ORIENTED_EDGE('',*,*,#1813,.F.);
#2282=ORIENTED_EDGE('',*,*,#1812,.T.);
#2283=ORIENTED_EDGE('',*,*,#1814,.T.);
#2284=ORIENTED_EDGE('',*,*,#1815,.F.);
#2285=ORIENTED_EDGE('',*,*,#1816,.F.);
#2286=ORIENTED_EDGE('',*,*,#1817,.T.);
#2287=ORIENTED_EDGE('',*,*,#1818,.T.);
#2288=ORIENTED_EDGE('',*,*,#1819,.T.);
#2289=ORIENTED_EDGE('',*,*,#1815,.T.);
#2290=ORIENTED_EDGE('',*,*,#1820,.T.);
#2291=ORIENTED_EDGE('',*,*,#1817,.F.);
#2292=ORIENTED_EDGE('',*,*,#1814,.F.);
#2293=ORIENTED_EDGE('',*,*,#1811,.T.);
#2294=ORIENTED_EDGE('',*,*,#1821,.F.);
#2295=ORIENTED_EDGE('',*,*,#1822,.F.);
#2296=ORIENTED_EDGE('',*,*,#1823,.T.);
#2297=ORIENTED_EDGE('',*,*,#1824,.F.);
#2298=ORIENTED_EDGE('',*,*,#1825,.T.);
#2299=ORIENTED_EDGE('',*,*,#1826,.T.);
#2300=ORIENTED_EDGE('',*,*,#1827,.T.);
#2301=ORIENTED_EDGE('',*,*,#1828,.T.);
#2302=ORIENTED_EDGE('',*,*,#1829,.T.);
#2303=ORIENTED_EDGE('',*,*,#1818,.F.);
#2304=ORIENTED_EDGE('',*,*,#1827,.F.);
#2305=ORIENTED_EDGE('',*,*,#1830,.F.);
#2306=ORIENTED_EDGE('',*,*,#1831,.F.);
#2307=ORIENTED_EDGE('',*,*,#1828,.F.);
#2308=ORIENTED_EDGE('',*,*,#1826,.F.);
#2309=ORIENTED_EDGE('',*,*,#1819,.F.);
#2310=ORIENTED_EDGE('',*,*,#1829,.F.);
#2311=ORIENTED_EDGE('',*,*,#1831,.T.);
#2312=ORIENTED_EDGE('',*,*,#1832,.F.);
#2313=ORIENTED_EDGE('',*,*,#1833,.F.);
#2314=ORIENTED_EDGE('',*,*,#1834,.T.);
#2315=ORIENTED_EDGE('',*,*,#1835,.F.);
#2316=ORIENTED_EDGE('',*,*,#1836,.T.);
#2317=ORIENTED_EDGE('',*,*,#1813,.T.);
#2318=ORIENTED_EDGE('',*,*,#1816,.T.);
#2319=ORIENTED_EDGE('',*,*,#1830,.T.);
#2320=ORIENTED_EDGE('',*,*,#1825,.F.);
#2321=ORIENTED_EDGE('',*,*,#1837,.F.);
#2322=ORIENTED_EDGE('',*,*,#1832,.T.);
#2323=ORIENTED_EDGE('',*,*,#1833,.T.);
#2324=ORIENTED_EDGE('',*,*,#1837,.T.);
#2325=ORIENTED_EDGE('',*,*,#1824,.T.);
#2326=ORIENTED_EDGE('',*,*,#1838,.T.);
#2327=ORIENTED_EDGE('',*,*,#1839,.T.);
#2328=ORIENTED_EDGE('',*,*,#1840,.T.);
#2329=ORIENTED_EDGE('',*,*,#1839,.F.);
#2330=ORIENTED_EDGE('',*,*,#1841,.F.);
#2331=ORIENTED_EDGE('',*,*,#1842,.T.);
#2332=ORIENTED_EDGE('',*,*,#1820,.F.);
#2333=ORIENTED_EDGE('',*,*,#1842,.F.);
#2334=ORIENTED_EDGE('',*,*,#1843,.F.);
#2335=ORIENTED_EDGE('',*,*,#1844,.F.);
#2336=ORIENTED_EDGE('',*,*,#1845,.F.);
#2337=ORIENTED_EDGE('',*,*,#1838,.F.);
#2338=ORIENTED_EDGE('',*,*,#1823,.F.);
#2339=ORIENTED_EDGE('',*,*,#1846,.F.);
#2340=ORIENTED_EDGE('',*,*,#1843,.T.);
#2341=ORIENTED_EDGE('',*,*,#1841,.T.);
#2342=ORIENTED_EDGE('',*,*,#1840,.F.);
#2343=ORIENTED_EDGE('',*,*,#1845,.T.);
#2344=ORIENTED_EDGE('',*,*,#1847,.F.);
#2345=ORIENTED_EDGE('',*,*,#1834,.F.);
#2346=ORIENTED_EDGE('',*,*,#1822,.T.);
#2347=ORIENTED_EDGE('',*,*,#1848,.T.);
#2348=ORIENTED_EDGE('',*,*,#1835,.T.);
#2349=ORIENTED_EDGE('',*,*,#1847,.T.);
#2350=ORIENTED_EDGE('',*,*,#1844,.T.);
#2351=ORIENTED_EDGE('',*,*,#1846,.T.);
#2352=ORIENTED_EDGE('',*,*,#1810,.T.);
#2353=ORIENTED_EDGE('',*,*,#1836,.F.);
#2354=ORIENTED_EDGE('',*,*,#1848,.F.);
#2355=ORIENTED_EDGE('',*,*,#1821,.T.);
#2356=ORIENTED_EDGE('',*,*,#1849,.T.);
#2357=ORIENTED_EDGE('',*,*,#1850,.T.);
#2358=ORIENTED_EDGE('',*,*,#1851,.T.);
#2359=ORIENTED_EDGE('',*,*,#1850,.F.);
#2360=ORIENTED_EDGE('',*,*,#1851,.F.);
#2361=ORIENTED_EDGE('',*,*,#1852,.T.);
#2362=ORIENTED_EDGE('',*,*,#1853,.T.);
#2363=ORIENTED_EDGE('',*,*,#1852,.F.);
#2364=ORIENTED_EDGE('',*,*,#1854,.T.);
#2365=ORIENTED_EDGE('',*,*,#1849,.F.);
#2366=ORIENTED_EDGE('',*,*,#1854,.F.);
#2367=ORIENTED_EDGE('',*,*,#1855,.T.);
#2368=ORIENTED_EDGE('',*,*,#1856,.T.);
#2369=ORIENTED_EDGE('',*,*,#1855,.F.);
#2370=ORIENTED_EDGE('',*,*,#1856,.F.);
#2371=ORIENTED_EDGE('',*,*,#1853,.F.);
#2372=ORIENTED_EDGE('',*,*,#1857,.T.);
#2373=ORIENTED_EDGE('',*,*,#1858,.F.);
#2374=ORIENTED_EDGE('',*,*,#1857,.F.);
#2375=ORIENTED_EDGE('',*,*,#1859,.T.);
#2376=ORIENTED_EDGE('',*,*,#1860,.T.);
#2377=ORIENTED_EDGE('',*,*,#1859,.F.);
#2378=ORIENTED_EDGE('',*,*,#1860,.F.);
#2379=ORIENTED_EDGE('',*,*,#1861,.F.);
#2380=ORIENTED_EDGE('',*,*,#1862,.F.);
#2381=ORIENTED_EDGE('',*,*,#1863,.T.);
#2382=ORIENTED_EDGE('',*,*,#1861,.T.);
#2383=ORIENTED_EDGE('',*,*,#1863,.F.);
#2384=ORIENTED_EDGE('',*,*,#1864,.F.);
#2385=ORIENTED_EDGE('',*,*,#1865,.T.);
#2386=ORIENTED_EDGE('',*,*,#1862,.T.);
#2387=ORIENTED_EDGE('',*,*,#1865,.F.);
#2388=ORIENTED_EDGE('',*,*,#1866,.F.);
#2389=ORIENTED_EDGE('',*,*,#1867,.T.);
#2390=ORIENTED_EDGE('',*,*,#1864,.T.);
#2391=ORIENTED_EDGE('',*,*,#1867,.F.);
#2392=ORIENTED_EDGE('',*,*,#1866,.T.);
#2393=ORIENTED_EDGE('',*,*,#1868,.F.);
#2394=ORIENTED_EDGE('',*,*,#1869,.F.);
#2395=ORIENTED_EDGE('',*,*,#1870,.T.);
#2396=ORIENTED_EDGE('',*,*,#1868,.T.);
#2397=ORIENTED_EDGE('',*,*,#1870,.F.);
#2398=ORIENTED_EDGE('',*,*,#1858,.T.);
#2399=ORIENTED_EDGE('',*,*,#1871,.T.);
#2400=ORIENTED_EDGE('',*,*,#1869,.T.);
#2401=ORIENTED_EDGE('',*,*,#1871,.F.);
#2402=ORIENTED_EDGE('',*,*,#1872,.T.);
#2403=ORIENTED_EDGE('',*,*,#1873,.T.);
#2404=ORIENTED_EDGE('',*,*,#1874,.T.);
#2405=ORIENTED_EDGE('',*,*,#1875,.F.);
#2406=ORIENTED_EDGE('',*,*,#1876,.T.);
#2407=ORIENTED_EDGE('',*,*,#1877,.T.);
#2408=ORIENTED_EDGE('',*,*,#1878,.T.);
#2409=ORIENTED_EDGE('',*,*,#1873,.F.);
#2410=ORIENTED_EDGE('',*,*,#1879,.T.);
#2411=ORIENTED_EDGE('',*,*,#1880,.T.);
#2412=ORIENTED_EDGE('',*,*,#1881,.T.);
#2413=ORIENTED_EDGE('',*,*,#1877,.F.);
#2414=ORIENTED_EDGE('',*,*,#1882,.T.);
#2415=ORIENTED_EDGE('',*,*,#1883,.T.);
#2416=ORIENTED_EDGE('',*,*,#1884,.T.);
#2417=ORIENTED_EDGE('',*,*,#1880,.F.);
#2418=ORIENTED_EDGE('',*,*,#1885,.T.);
#2419=ORIENTED_EDGE('',*,*,#1886,.T.);
#2420=ORIENTED_EDGE('',*,*,#1887,.T.);
#2421=ORIENTED_EDGE('',*,*,#1883,.F.);
#2422=ORIENTED_EDGE('',*,*,#1888,.T.);
#2423=ORIENTED_EDGE('',*,*,#1875,.T.);
#2424=ORIENTED_EDGE('',*,*,#1889,.T.);
#2425=ORIENTED_EDGE('',*,*,#1886,.F.);
#2426=ORIENTED_EDGE('',*,*,#1888,.F.);
#2427=ORIENTED_EDGE('',*,*,#1885,.F.);
#2428=ORIENTED_EDGE('',*,*,#1882,.F.);
#2429=ORIENTED_EDGE('',*,*,#1879,.F.);
#2430=ORIENTED_EDGE('',*,*,#1876,.F.);
#2431=ORIENTED_EDGE('',*,*,#1872,.F.);
#2432=ORIENTED_EDGE('',*,*,#1889,.F.);
#2433=ORIENTED_EDGE('',*,*,#1874,.F.);
#2434=ORIENTED_EDGE('',*,*,#1878,.F.);
#2435=ORIENTED_EDGE('',*,*,#1881,.F.);
#2436=ORIENTED_EDGE('',*,*,#1884,.F.);
#2437=ORIENTED_EDGE('',*,*,#1887,.F.);
#2438=ORIENTED_EDGE('',*,*,#1890,.F.);
#2439=ORIENTED_EDGE('',*,*,#1891,.T.);
#2440=ORIENTED_EDGE('',*,*,#1892,.F.);
#2441=ORIENTED_EDGE('',*,*,#1893,.F.);
#2442=ORIENTED_EDGE('',*,*,#1894,.F.);
#2443=ORIENTED_EDGE('',*,*,#1895,.T.);
#2444=ORIENTED_EDGE('',*,*,#1896,.F.);
#2445=ORIENTED_EDGE('',*,*,#1891,.F.);
#2446=ORIENTED_EDGE('',*,*,#1897,.F.);
#2447=ORIENTED_EDGE('',*,*,#1898,.T.);
#2448=ORIENTED_EDGE('',*,*,#1899,.F.);
#2449=ORIENTED_EDGE('',*,*,#1895,.F.);
#2450=ORIENTED_EDGE('',*,*,#1900,.F.);
#2451=ORIENTED_EDGE('',*,*,#1901,.T.);
#2452=ORIENTED_EDGE('',*,*,#1902,.F.);
#2453=ORIENTED_EDGE('',*,*,#1898,.F.);
#2454=ORIENTED_EDGE('',*,*,#1903,.F.);
#2455=ORIENTED_EDGE('',*,*,#1904,.T.);
#2456=ORIENTED_EDGE('',*,*,#1905,.F.);
#2457=ORIENTED_EDGE('',*,*,#1901,.F.);
#2458=ORIENTED_EDGE('',*,*,#1906,.F.);
#2459=ORIENTED_EDGE('',*,*,#1907,.T.);
#2460=ORIENTED_EDGE('',*,*,#1908,.F.);
#2461=ORIENTED_EDGE('',*,*,#1904,.F.);
#2462=ORIENTED_EDGE('',*,*,#1909,.F.);
#2463=ORIENTED_EDGE('',*,*,#1910,.T.);
#2464=ORIENTED_EDGE('',*,*,#1911,.F.);
#2465=ORIENTED_EDGE('',*,*,#1907,.F.);
#2466=ORIENTED_EDGE('',*,*,#1912,.F.);
#2467=ORIENTED_EDGE('',*,*,#1913,.T.);
#2468=ORIENTED_EDGE('',*,*,#1914,.F.);
#2469=ORIENTED_EDGE('',*,*,#1910,.F.);
#2470=ORIENTED_EDGE('',*,*,#1915,.F.);
#2471=ORIENTED_EDGE('',*,*,#1916,.F.);
#2472=ORIENTED_EDGE('',*,*,#1917,.F.);
#2473=ORIENTED_EDGE('',*,*,#1913,.F.);
#2474=ORIENTED_EDGE('',*,*,#1918,.F.);
#2475=ORIENTED_EDGE('',*,*,#1919,.T.);
#2476=ORIENTED_EDGE('',*,*,#1920,.F.);
#2477=ORIENTED_EDGE('',*,*,#1921,.F.);
#2478=ORIENTED_EDGE('',*,*,#1922,.F.);
#2479=ORIENTED_EDGE('',*,*,#1923,.T.);
#2480=ORIENTED_EDGE('',*,*,#1924,.F.);
#2481=ORIENTED_EDGE('',*,*,#1919,.F.);
#2482=ORIENTED_EDGE('',*,*,#1925,.F.);
#2483=ORIENTED_EDGE('',*,*,#1926,.T.);
#2484=ORIENTED_EDGE('',*,*,#1927,.F.);
#2485=ORIENTED_EDGE('',*,*,#1923,.F.);
#2486=ORIENTED_EDGE('',*,*,#1928,.F.);
#2487=ORIENTED_EDGE('',*,*,#1929,.T.);
#2488=ORIENTED_EDGE('',*,*,#1930,.F.);
#2489=ORIENTED_EDGE('',*,*,#1926,.F.);
#2490=ORIENTED_EDGE('',*,*,#1931,.F.);
#2491=ORIENTED_EDGE('',*,*,#1932,.T.);
#2492=ORIENTED_EDGE('',*,*,#1933,.F.);
#2493=ORIENTED_EDGE('',*,*,#1929,.F.);
#2494=ORIENTED_EDGE('',*,*,#1934,.F.);
#2495=ORIENTED_EDGE('',*,*,#1935,.T.);
#2496=ORIENTED_EDGE('',*,*,#1936,.F.);
#2497=ORIENTED_EDGE('',*,*,#1932,.F.);
#2498=ORIENTED_EDGE('',*,*,#1937,.F.);
#2499=ORIENTED_EDGE('',*,*,#1938,.T.);
#2500=ORIENTED_EDGE('',*,*,#1939,.F.);
#2501=ORIENTED_EDGE('',*,*,#1935,.F.);
#2502=ORIENTED_EDGE('',*,*,#1940,.F.);
#2503=ORIENTED_EDGE('',*,*,#1941,.T.);
#2504=ORIENTED_EDGE('',*,*,#1942,.F.);
#2505=ORIENTED_EDGE('',*,*,#1938,.F.);
#2506=ORIENTED_EDGE('',*,*,#1943,.F.);
#2507=ORIENTED_EDGE('',*,*,#1944,.F.);
#2508=ORIENTED_EDGE('',*,*,#1945,.F.);
#2509=ORIENTED_EDGE('',*,*,#1941,.F.);
#2510=ORIENTED_EDGE('',*,*,#1946,.F.);
#2511=ORIENTED_EDGE('',*,*,#1947,.T.);
#2512=ORIENTED_EDGE('',*,*,#1948,.F.);
#2513=ORIENTED_EDGE('',*,*,#1949,.F.);
#2514=ORIENTED_EDGE('',*,*,#1950,.F.);
#2515=ORIENTED_EDGE('',*,*,#1951,.T.);
#2516=ORIENTED_EDGE('',*,*,#1952,.F.);
#2517=ORIENTED_EDGE('',*,*,#1947,.F.);
#2518=ORIENTED_EDGE('',*,*,#1953,.F.);
#2519=ORIENTED_EDGE('',*,*,#1954,.T.);
#2520=ORIENTED_EDGE('',*,*,#1955,.F.);
#2521=ORIENTED_EDGE('',*,*,#1951,.F.);
#2522=ORIENTED_EDGE('',*,*,#1956,.F.);
#2523=ORIENTED_EDGE('',*,*,#1957,.T.);
#2524=ORIENTED_EDGE('',*,*,#1958,.F.);
#2525=ORIENTED_EDGE('',*,*,#1954,.F.);
#2526=ORIENTED_EDGE('',*,*,#1959,.F.);
#2527=ORIENTED_EDGE('',*,*,#1960,.T.);
#2528=ORIENTED_EDGE('',*,*,#1961,.F.);
#2529=ORIENTED_EDGE('',*,*,#1957,.F.);
#2530=ORIENTED_EDGE('',*,*,#1962,.F.);
#2531=ORIENTED_EDGE('',*,*,#1963,.T.);
#2532=ORIENTED_EDGE('',*,*,#1964,.F.);
#2533=ORIENTED_EDGE('',*,*,#1960,.F.);
#2534=ORIENTED_EDGE('',*,*,#1965,.F.);
#2535=ORIENTED_EDGE('',*,*,#1966,.T.);
#2536=ORIENTED_EDGE('',*,*,#1967,.F.);
#2537=ORIENTED_EDGE('',*,*,#1963,.F.);
#2538=ORIENTED_EDGE('',*,*,#1968,.F.);
#2539=ORIENTED_EDGE('',*,*,#1969,.T.);
#2540=ORIENTED_EDGE('',*,*,#1970,.F.);
#2541=ORIENTED_EDGE('',*,*,#1966,.F.);
#2542=ORIENTED_EDGE('',*,*,#1971,.F.);
#2543=ORIENTED_EDGE('',*,*,#1972,.F.);
#2544=ORIENTED_EDGE('',*,*,#1973,.F.);
#2545=ORIENTED_EDGE('',*,*,#1969,.F.);
#2546=ORIENTED_EDGE('',*,*,#1974,.F.);
#2547=ORIENTED_EDGE('',*,*,#1975,.T.);
#2548=ORIENTED_EDGE('',*,*,#1976,.F.);
#2549=ORIENTED_EDGE('',*,*,#1977,.F.);
#2550=ORIENTED_EDGE('',*,*,#1978,.F.);
#2551=ORIENTED_EDGE('',*,*,#1979,.T.);
#2552=ORIENTED_EDGE('',*,*,#1980,.F.);
#2553=ORIENTED_EDGE('',*,*,#1975,.F.);
#2554=ORIENTED_EDGE('',*,*,#1981,.F.);
#2555=ORIENTED_EDGE('',*,*,#1982,.T.);
#2556=ORIENTED_EDGE('',*,*,#1983,.F.);
#2557=ORIENTED_EDGE('',*,*,#1979,.F.);
#2558=ORIENTED_EDGE('',*,*,#1984,.F.);
#2559=ORIENTED_EDGE('',*,*,#1985,.T.);
#2560=ORIENTED_EDGE('',*,*,#1986,.F.);
#2561=ORIENTED_EDGE('',*,*,#1982,.F.);
#2562=ORIENTED_EDGE('',*,*,#1987,.F.);
#2563=ORIENTED_EDGE('',*,*,#1988,.T.);
#2564=ORIENTED_EDGE('',*,*,#1989,.F.);
#2565=ORIENTED_EDGE('',*,*,#1985,.F.);
#2566=ORIENTED_EDGE('',*,*,#1990,.F.);
#2567=ORIENTED_EDGE('',*,*,#1991,.T.);
#2568=ORIENTED_EDGE('',*,*,#1992,.F.);
#2569=ORIENTED_EDGE('',*,*,#1988,.F.);
#2570=ORIENTED_EDGE('',*,*,#1993,.F.);
#2571=ORIENTED_EDGE('',*,*,#1994,.T.);
#2572=ORIENTED_EDGE('',*,*,#1995,.F.);
#2573=ORIENTED_EDGE('',*,*,#1991,.F.);
#2574=ORIENTED_EDGE('',*,*,#1996,.F.);
#2575=ORIENTED_EDGE('',*,*,#1997,.T.);
#2576=ORIENTED_EDGE('',*,*,#1998,.F.);
#2577=ORIENTED_EDGE('',*,*,#1994,.F.);
#2578=ORIENTED_EDGE('',*,*,#1999,.F.);
#2579=ORIENTED_EDGE('',*,*,#2000,.F.);
#2580=ORIENTED_EDGE('',*,*,#2001,.F.);
#2581=ORIENTED_EDGE('',*,*,#1997,.F.);
#2582=ORIENTED_EDGE('',*,*,#2002,.F.);
#2583=ORIENTED_EDGE('',*,*,#2003,.T.);
#2584=ORIENTED_EDGE('',*,*,#2004,.F.);
#2585=ORIENTED_EDGE('',*,*,#2003,.F.);
#2586=ORIENTED_EDGE('',*,*,#1916,.T.);
#2587=ORIENTED_EDGE('',*,*,#2005,.T.);
#2588=ORIENTED_EDGE('',*,*,#2006,.T.);
#2589=ORIENTED_EDGE('',*,*,#2007,.F.);
#2590=ORIENTED_EDGE('',*,*,#1893,.T.);
#2591=ORIENTED_EDGE('',*,*,#2008,.F.);
#2592=ORIENTED_EDGE('',*,*,#2009,.F.);
#2593=ORIENTED_EDGE('',*,*,#2010,.T.);
#2594=ORIENTED_EDGE('',*,*,#1944,.T.);
#2595=ORIENTED_EDGE('',*,*,#2011,.T.);
#2596=ORIENTED_EDGE('',*,*,#2009,.T.);
#2597=ORIENTED_EDGE('',*,*,#2012,.F.);
#2598=ORIENTED_EDGE('',*,*,#1921,.T.);
#2599=ORIENTED_EDGE('',*,*,#2013,.F.);
#2600=ORIENTED_EDGE('',*,*,#2014,.F.);
#2601=ORIENTED_EDGE('',*,*,#2015,.T.);
#2602=ORIENTED_EDGE('',*,*,#1972,.T.);
#2603=ORIENTED_EDGE('',*,*,#2016,.T.);
#2604=ORIENTED_EDGE('',*,*,#2014,.T.);
#2605=ORIENTED_EDGE('',*,*,#2017,.F.);
#2606=ORIENTED_EDGE('',*,*,#1949,.T.);
#2607=ORIENTED_EDGE('',*,*,#2018,.F.);
#2608=ORIENTED_EDGE('',*,*,#2019,.F.);
#2609=ORIENTED_EDGE('',*,*,#2020,.T.);
#2610=ORIENTED_EDGE('',*,*,#2000,.T.);
#2611=ORIENTED_EDGE('',*,*,#2021,.T.);
#2612=ORIENTED_EDGE('',*,*,#2019,.T.);
#2613=ORIENTED_EDGE('',*,*,#2022,.F.);
#2614=ORIENTED_EDGE('',*,*,#1977,.T.);
#2615=ORIENTED_EDGE('',*,*,#2023,.F.);
#2616=ORIENTED_EDGE('',*,*,#2006,.F.);
#2617=ORIENTED_EDGE('',*,*,#2024,.T.);
#2618=ORIENTED_EDGE('',*,*,#1892,.T.);
#2619=ORIENTED_EDGE('',*,*,#1896,.T.);
#2620=ORIENTED_EDGE('',*,*,#1899,.T.);
#2621=ORIENTED_EDGE('',*,*,#1902,.T.);
#2622=ORIENTED_EDGE('',*,*,#1905,.T.);
#2623=ORIENTED_EDGE('',*,*,#1908,.T.);
#2624=ORIENTED_EDGE('',*,*,#1911,.T.);
#2625=ORIENTED_EDGE('',*,*,#1914,.T.);
#2626=ORIENTED_EDGE('',*,*,#1917,.T.);
#2627=ORIENTED_EDGE('',*,*,#2007,.T.);
#2628=ORIENTED_EDGE('',*,*,#2023,.T.);
#2629=ORIENTED_EDGE('',*,*,#1976,.T.);
#2630=ORIENTED_EDGE('',*,*,#1980,.T.);
#2631=ORIENTED_EDGE('',*,*,#1983,.T.);
#2632=ORIENTED_EDGE('',*,*,#1986,.T.);
#2633=ORIENTED_EDGE('',*,*,#1989,.T.);
#2634=ORIENTED_EDGE('',*,*,#1992,.T.);
#2635=ORIENTED_EDGE('',*,*,#1995,.T.);
#2636=ORIENTED_EDGE('',*,*,#1998,.T.);
#2637=ORIENTED_EDGE('',*,*,#2001,.T.);
#2638=ORIENTED_EDGE('',*,*,#2022,.T.);
#2639=ORIENTED_EDGE('',*,*,#2018,.T.);
#2640=ORIENTED_EDGE('',*,*,#1948,.T.);
#2641=ORIENTED_EDGE('',*,*,#1952,.T.);
#2642=ORIENTED_EDGE('',*,*,#1955,.T.);
#2643=ORIENTED_EDGE('',*,*,#1958,.T.);
#2644=ORIENTED_EDGE('',*,*,#1961,.T.);
#2645=ORIENTED_EDGE('',*,*,#1964,.T.);
#2646=ORIENTED_EDGE('',*,*,#1967,.T.);
#2647=ORIENTED_EDGE('',*,*,#1970,.T.);
#2648=ORIENTED_EDGE('',*,*,#1973,.T.);
#2649=ORIENTED_EDGE('',*,*,#2017,.T.);
#2650=ORIENTED_EDGE('',*,*,#2013,.T.);
#2651=ORIENTED_EDGE('',*,*,#1920,.T.);
#2652=ORIENTED_EDGE('',*,*,#1924,.T.);
#2653=ORIENTED_EDGE('',*,*,#1927,.T.);
#2654=ORIENTED_EDGE('',*,*,#1930,.T.);
#2655=ORIENTED_EDGE('',*,*,#1933,.T.);
#2656=ORIENTED_EDGE('',*,*,#1936,.T.);
#2657=ORIENTED_EDGE('',*,*,#1939,.T.);
#2658=ORIENTED_EDGE('',*,*,#1942,.T.);
#2659=ORIENTED_EDGE('',*,*,#1945,.T.);
#2660=ORIENTED_EDGE('',*,*,#2012,.T.);
#2661=ORIENTED_EDGE('',*,*,#2008,.T.);
#2662=ORIENTED_EDGE('',*,*,#2004,.T.);
#2663=ORIENTED_EDGE('',*,*,#1890,.T.);
#2664=ORIENTED_EDGE('',*,*,#2010,.F.);
#2665=ORIENTED_EDGE('',*,*,#2011,.F.);
#2666=ORIENTED_EDGE('',*,*,#1943,.T.);
#2667=ORIENTED_EDGE('',*,*,#1940,.T.);
#2668=ORIENTED_EDGE('',*,*,#1937,.T.);
#2669=ORIENTED_EDGE('',*,*,#1934,.T.);
#2670=ORIENTED_EDGE('',*,*,#1931,.T.);
#2671=ORIENTED_EDGE('',*,*,#1928,.T.);
#2672=ORIENTED_EDGE('',*,*,#1925,.T.);
#2673=ORIENTED_EDGE('',*,*,#1922,.T.);
#2674=ORIENTED_EDGE('',*,*,#1918,.T.);
#2675=ORIENTED_EDGE('',*,*,#2015,.F.);
#2676=ORIENTED_EDGE('',*,*,#2016,.F.);
#2677=ORIENTED_EDGE('',*,*,#1971,.T.);
#2678=ORIENTED_EDGE('',*,*,#1968,.T.);
#2679=ORIENTED_EDGE('',*,*,#1965,.T.);
#2680=ORIENTED_EDGE('',*,*,#1962,.T.);
#2681=ORIENTED_EDGE('',*,*,#1959,.T.);
#2682=ORIENTED_EDGE('',*,*,#1956,.T.);
#2683=ORIENTED_EDGE('',*,*,#1953,.T.);
#2684=ORIENTED_EDGE('',*,*,#1950,.T.);
#2685=ORIENTED_EDGE('',*,*,#1946,.T.);
#2686=ORIENTED_EDGE('',*,*,#2020,.F.);
#2687=ORIENTED_EDGE('',*,*,#2021,.F.);
#2688=ORIENTED_EDGE('',*,*,#1999,.T.);
#2689=ORIENTED_EDGE('',*,*,#1996,.T.);
#2690=ORIENTED_EDGE('',*,*,#1993,.T.);
#2691=ORIENTED_EDGE('',*,*,#1990,.T.);
#2692=ORIENTED_EDGE('',*,*,#1987,.T.);
#2693=ORIENTED_EDGE('',*,*,#1984,.T.);
#2694=ORIENTED_EDGE('',*,*,#1981,.T.);
#2695=ORIENTED_EDGE('',*,*,#1978,.T.);
#2696=ORIENTED_EDGE('',*,*,#1974,.T.);
#2697=ORIENTED_EDGE('',*,*,#2024,.F.);
#2698=ORIENTED_EDGE('',*,*,#2005,.F.);
#2699=ORIENTED_EDGE('',*,*,#1915,.T.);
#2700=ORIENTED_EDGE('',*,*,#1912,.T.);
#2701=ORIENTED_EDGE('',*,*,#1909,.T.);
#2702=ORIENTED_EDGE('',*,*,#1906,.T.);
#2703=ORIENTED_EDGE('',*,*,#1903,.T.);
#2704=ORIENTED_EDGE('',*,*,#1900,.T.);
#2705=ORIENTED_EDGE('',*,*,#1897,.T.);
#2706=ORIENTED_EDGE('',*,*,#1894,.T.);
#2707=ORIENTED_EDGE('',*,*,#2002,.T.);
#2708=ORIENTED_EDGE('',*,*,#2025,.F.);
#2709=ORIENTED_EDGE('',*,*,#2026,.T.);
#2710=ORIENTED_EDGE('',*,*,#2027,.F.);
#2711=ORIENTED_EDGE('',*,*,#2026,.F.);
#2712=ORIENTED_EDGE('',*,*,#2028,.F.);
#2713=ORIENTED_EDGE('',*,*,#2029,.T.);
#2714=ORIENTED_EDGE('',*,*,#2025,.T.);
#2715=ORIENTED_EDGE('',*,*,#2029,.F.);
#2716=ORIENTED_EDGE('',*,*,#2028,.T.);
#2717=ORIENTED_EDGE('',*,*,#2030,.F.);
#2718=ORIENTED_EDGE('',*,*,#2031,.T.);
#2719=ORIENTED_EDGE('',*,*,#2032,.F.);
#2720=ORIENTED_EDGE('',*,*,#2033,.F.);
#2721=ORIENTED_EDGE('',*,*,#2034,.F.);
#2722=ORIENTED_EDGE('',*,*,#2035,.F.);
#2723=ORIENTED_EDGE('',*,*,#2036,.F.);
#2724=ORIENTED_EDGE('',*,*,#2037,.F.);
#2725=ORIENTED_EDGE('',*,*,#2031,.F.);
#2726=ORIENTED_EDGE('',*,*,#2036,.T.);
#2727=ORIENTED_EDGE('',*,*,#2038,.F.);
#2728=ORIENTED_EDGE('',*,*,#2039,.T.);
#2729=ORIENTED_EDGE('',*,*,#2040,.T.);
#2730=ORIENTED_EDGE('',*,*,#2035,.T.);
#2731=ORIENTED_EDGE('',*,*,#2041,.F.);
#2732=ORIENTED_EDGE('',*,*,#2042,.T.);
#2733=ORIENTED_EDGE('',*,*,#2038,.T.);
#2734=ORIENTED_EDGE('',*,*,#2034,.T.);
#2735=ORIENTED_EDGE('',*,*,#2043,.F.);
#2736=ORIENTED_EDGE('',*,*,#2044,.T.);
#2737=ORIENTED_EDGE('',*,*,#2041,.T.);
#2738=ORIENTED_EDGE('',*,*,#2033,.T.);
#2739=ORIENTED_EDGE('',*,*,#2045,.F.);
#2740=ORIENTED_EDGE('',*,*,#2046,.T.);
#2741=ORIENTED_EDGE('',*,*,#2043,.T.);
#2742=ORIENTED_EDGE('',*,*,#2032,.T.);
#2743=ORIENTED_EDGE('',*,*,#2047,.F.);
#2744=ORIENTED_EDGE('',*,*,#2048,.T.);
#2745=ORIENTED_EDGE('',*,*,#2045,.T.);
#2746=ORIENTED_EDGE('',*,*,#2037,.T.);
#2747=ORIENTED_EDGE('',*,*,#2040,.F.);
#2748=ORIENTED_EDGE('',*,*,#2049,.T.);
#2749=ORIENTED_EDGE('',*,*,#2047,.T.);
#2750=ORIENTED_EDGE('',*,*,#2030,.T.);
#2751=ORIENTED_EDGE('',*,*,#2044,.F.);
#2752=ORIENTED_EDGE('',*,*,#2046,.F.);
#2753=ORIENTED_EDGE('',*,*,#2048,.F.);
#2754=ORIENTED_EDGE('',*,*,#2049,.F.);
#2755=ORIENTED_EDGE('',*,*,#2039,.F.);
#2756=ORIENTED_EDGE('',*,*,#2042,.F.);
#2757=ORIENTED_EDGE('',*,*,#2027,.T.);
#2758=ORIENTED_EDGE('',*,*,#2050,.F.);
#2759=ORIENTED_EDGE('',*,*,#2051,.T.);
#2760=ORIENTED_EDGE('',*,*,#2052,.F.);
#2761=ORIENTED_EDGE('',*,*,#2051,.F.);
#2762=ORIENTED_EDGE('',*,*,#2053,.F.);
#2763=ORIENTED_EDGE('',*,*,#2054,.T.);
#2764=ORIENTED_EDGE('',*,*,#2055,.F.);
#2765=ORIENTED_EDGE('',*,*,#2054,.F.);
#2766=ORIENTED_EDGE('',*,*,#2056,.T.);
#2767=ORIENTED_EDGE('',*,*,#2057,.T.);
#2768=ORIENTED_EDGE('',*,*,#2058,.T.);
#2769=ORIENTED_EDGE('',*,*,#2059,.T.);
#2770=ORIENTED_EDGE('',*,*,#2060,.T.);
#2771=ORIENTED_EDGE('',*,*,#2052,.T.);
#2772=ORIENTED_EDGE('',*,*,#2055,.T.);
#2773=ORIENTED_EDGE('',*,*,#2061,.T.);
#2774=ORIENTED_EDGE('',*,*,#2062,.F.);
#2775=ORIENTED_EDGE('',*,*,#2060,.F.);
#2776=ORIENTED_EDGE('',*,*,#2063,.F.);
#2777=ORIENTED_EDGE('',*,*,#2064,.T.);
#2778=ORIENTED_EDGE('',*,*,#2065,.T.);
#2779=ORIENTED_EDGE('',*,*,#2063,.T.);
#2780=ORIENTED_EDGE('',*,*,#2059,.F.);
#2781=ORIENTED_EDGE('',*,*,#2066,.F.);
#2782=ORIENTED_EDGE('',*,*,#2067,.F.);
#2783=ORIENTED_EDGE('',*,*,#2068,.T.);
#2784=ORIENTED_EDGE('',*,*,#2066,.T.);
#2785=ORIENTED_EDGE('',*,*,#2058,.F.);
#2786=ORIENTED_EDGE('',*,*,#2069,.F.);
#2787=ORIENTED_EDGE('',*,*,#2064,.F.);
#2788=ORIENTED_EDGE('',*,*,#2065,.F.);
#2789=ORIENTED_EDGE('',*,*,#2068,.F.);
#2790=ORIENTED_EDGE('',*,*,#2050,.T.);
#2791=ORIENTED_EDGE('',*,*,#2053,.T.);
#2792=ORIENTED_EDGE('',*,*,#2062,.T.);
#2793=ORIENTED_EDGE('',*,*,#2069,.T.);
#2794=ORIENTED_EDGE('',*,*,#2067,.T.);
#2795=ORIENTED_EDGE('',*,*,#2057,.F.);
#2796=ORIENTED_EDGE('',*,*,#2070,.T.);
#2797=ORIENTED_EDGE('',*,*,#2071,.T.);
#2798=ORIENTED_EDGE('',*,*,#2070,.F.);
#2799=ORIENTED_EDGE('',*,*,#2056,.F.);
#2800=ORIENTED_EDGE('',*,*,#2061,.F.);
#2801=ORIENTED_EDGE('',*,*,#2072,.T.);
#2802=ORIENTED_EDGE('',*,*,#2073,.T.);
#2803=ORIENTED_EDGE('',*,*,#2072,.F.);
#2804=ORIENTED_EDGE('',*,*,#2071,.F.);
#2805=ORIENTED_EDGE('',*,*,#2073,.F.);
#2806=ORIENTED_EDGE('',*,*,#2074,.F.);
#2807=ORIENTED_EDGE('',*,*,#2075,.T.);
#2808=ORIENTED_EDGE('',*,*,#2076,.F.);
#2809=ORIENTED_EDGE('',*,*,#2075,.F.);
#2810=ORIENTED_EDGE('',*,*,#2074,.T.);
#2811=ORIENTED_EDGE('',*,*,#2077,.F.);
#2812=ORIENTED_EDGE('',*,*,#2078,.F.);
#2813=ORIENTED_EDGE('',*,*,#2079,.T.);
#2814=ORIENTED_EDGE('',*,*,#2080,.F.);
#2815=ORIENTED_EDGE('',*,*,#2079,.F.);
#2816=ORIENTED_EDGE('',*,*,#2078,.T.);
#2817=ORIENTED_EDGE('',*,*,#2081,.F.);
#2818=ORIENTED_EDGE('',*,*,#2082,.F.);
#2819=ORIENTED_EDGE('',*,*,#2083,.T.);
#2820=ORIENTED_EDGE('',*,*,#2077,.T.);
#2821=ORIENTED_EDGE('',*,*,#2083,.F.);
#2822=ORIENTED_EDGE('',*,*,#2084,.F.);
#2823=ORIENTED_EDGE('',*,*,#2085,.T.);
#2824=ORIENTED_EDGE('',*,*,#2081,.T.);
#2825=ORIENTED_EDGE('',*,*,#2085,.F.);
#2826=ORIENTED_EDGE('',*,*,#2086,.T.);
#2827=ORIENTED_EDGE('',*,*,#2087,.T.);
#2828=ORIENTED_EDGE('',*,*,#2088,.F.);
#2829=ORIENTED_EDGE('',*,*,#2089,.F.);
#2830=ORIENTED_EDGE('',*,*,#2090,.T.);
#2831=ORIENTED_EDGE('',*,*,#2089,.T.);
#2832=ORIENTED_EDGE('',*,*,#2091,.F.);
#2833=ORIENTED_EDGE('',*,*,#2092,.F.);
#2834=ORIENTED_EDGE('',*,*,#2093,.T.);
#2835=ORIENTED_EDGE('',*,*,#2092,.T.);
#2836=ORIENTED_EDGE('',*,*,#2094,.F.);
#2837=ORIENTED_EDGE('',*,*,#2095,.F.);
#2838=ORIENTED_EDGE('',*,*,#2096,.T.);
#2839=ORIENTED_EDGE('',*,*,#2095,.T.);
#2840=ORIENTED_EDGE('',*,*,#2097,.F.);
#2841=ORIENTED_EDGE('',*,*,#2087,.F.);
#2842=ORIENTED_EDGE('',*,*,#2097,.T.);
#2843=ORIENTED_EDGE('',*,*,#2094,.T.);
#2844=ORIENTED_EDGE('',*,*,#2091,.T.);
#2845=ORIENTED_EDGE('',*,*,#2088,.T.);
#2846=ORIENTED_EDGE('',*,*,#2076,.T.);
#2847=ORIENTED_EDGE('',*,*,#2080,.T.);
#2848=ORIENTED_EDGE('',*,*,#2096,.F.);
#2849=ORIENTED_EDGE('',*,*,#2086,.F.);
#2850=ORIENTED_EDGE('',*,*,#2090,.F.);
#2851=ORIENTED_EDGE('',*,*,#2093,.F.);
#2852=ORIENTED_EDGE('',*,*,#2082,.T.);
#2853=ORIENTED_EDGE('',*,*,#2084,.T.);
#2854=ORIENTED_EDGE('',*,*,#2098,.F.);
#2855=ORIENTED_EDGE('',*,*,#2099,.F.);
#2856=ORIENTED_EDGE('',*,*,#2100,.T.);
#2857=ORIENTED_EDGE('',*,*,#2098,.T.);
#2858=ORIENTED_EDGE('',*,*,#2100,.F.);
#2859=ORIENTED_EDGE('',*,*,#2101,.F.);
#2860=ORIENTED_EDGE('',*,*,#2102,.T.);
#2861=ORIENTED_EDGE('',*,*,#2099,.T.);
#2862=ORIENTED_EDGE('',*,*,#2102,.F.);
#2863=ORIENTED_EDGE('',*,*,#2103,.F.);
#2864=ORIENTED_EDGE('',*,*,#2104,.T.);
#2865=ORIENTED_EDGE('',*,*,#2101,.T.);
#2866=ORIENTED_EDGE('',*,*,#2104,.F.);
#2867=ORIENTED_EDGE('',*,*,#2103,.T.);
#2868=ORIENTED_EDGE('',*,*,#2105,.F.);
#2869=ORIENTED_EDGE('',*,*,#2106,.F.);
#2870=ORIENTED_EDGE('',*,*,#2107,.T.);
#2871=ORIENTED_EDGE('',*,*,#2105,.T.);
#2872=ORIENTED_EDGE('',*,*,#2107,.F.);
#2873=ORIENTED_EDGE('',*,*,#2108,.F.);
#2874=ORIENTED_EDGE('',*,*,#2109,.T.);
#2875=ORIENTED_EDGE('',*,*,#2106,.T.);
#2876=ORIENTED_EDGE('',*,*,#2109,.F.);
#2877=ORIENTED_EDGE('',*,*,#2110,.F.);
#2878=ORIENTED_EDGE('',*,*,#2111,.T.);
#2879=ORIENTED_EDGE('',*,*,#2108,.T.);
#2880=ORIENTED_EDGE('',*,*,#2111,.F.);
#2881=ORIENTED_EDGE('',*,*,#2110,.T.);
#2882=ORIENTED_EDGE('',*,*,#2112,.T.);
#2883=ORIENTED_EDGE('',*,*,#2113,.T.);
#2884=ORIENTED_EDGE('',*,*,#2114,.T.);
#2885=ORIENTED_EDGE('',*,*,#2115,.F.);
#2886=ORIENTED_EDGE('',*,*,#2116,.T.);
#2887=ORIENTED_EDGE('',*,*,#2117,.T.);
#2888=ORIENTED_EDGE('',*,*,#2118,.T.);
#2889=ORIENTED_EDGE('',*,*,#2113,.F.);
#2890=ORIENTED_EDGE('',*,*,#2119,.T.);
#2891=ORIENTED_EDGE('',*,*,#2120,.T.);
#2892=ORIENTED_EDGE('',*,*,#2121,.T.);
#2893=ORIENTED_EDGE('',*,*,#2117,.F.);
#2894=ORIENTED_EDGE('',*,*,#2122,.T.);
#2895=ORIENTED_EDGE('',*,*,#2123,.T.);
#2896=ORIENTED_EDGE('',*,*,#2124,.T.);
#2897=ORIENTED_EDGE('',*,*,#2120,.F.);
#2898=ORIENTED_EDGE('',*,*,#2125,.T.);
#2899=ORIENTED_EDGE('',*,*,#2126,.T.);
#2900=ORIENTED_EDGE('',*,*,#2127,.T.);
#2901=ORIENTED_EDGE('',*,*,#2123,.F.);
#2902=ORIENTED_EDGE('',*,*,#2128,.T.);
#2903=ORIENTED_EDGE('',*,*,#2115,.T.);
#2904=ORIENTED_EDGE('',*,*,#2129,.T.);
#2905=ORIENTED_EDGE('',*,*,#2126,.F.);
#2906=ORIENTED_EDGE('',*,*,#2128,.F.);
#2907=ORIENTED_EDGE('',*,*,#2125,.F.);
#2908=ORIENTED_EDGE('',*,*,#2122,.F.);
#2909=ORIENTED_EDGE('',*,*,#2119,.F.);
#2910=ORIENTED_EDGE('',*,*,#2116,.F.);
#2911=ORIENTED_EDGE('',*,*,#2112,.F.);
#2912=ORIENTED_EDGE('',*,*,#2129,.F.);
#2913=ORIENTED_EDGE('',*,*,#2114,.F.);
#2914=ORIENTED_EDGE('',*,*,#2118,.F.);
#2915=ORIENTED_EDGE('',*,*,#2121,.F.);
#2916=ORIENTED_EDGE('',*,*,#2124,.F.);
#2917=ORIENTED_EDGE('',*,*,#2127,.F.);
#2918=ORIENTED_EDGE('',*,*,#2130,.F.);
#2919=ORIENTED_EDGE('',*,*,#2131,.T.);
#2920=ORIENTED_EDGE('',*,*,#2132,.T.);
#2921=ORIENTED_EDGE('',*,*,#2131,.F.);
#2922=ORIENTED_EDGE('',*,*,#2133,.F.);
#2923=ORIENTED_EDGE('',*,*,#2134,.T.);
#2924=ORIENTED_EDGE('',*,*,#2135,.T.);
#2925=ORIENTED_EDGE('',*,*,#2134,.F.);
#2926=ORIENTED_EDGE('',*,*,#2133,.T.);
#2927=ORIENTED_EDGE('',*,*,#2130,.T.);
#2928=ORIENTED_EDGE('',*,*,#2135,.F.);
#2929=ORIENTED_EDGE('',*,*,#2132,.F.);
#2930=ORIENTED_EDGE('',*,*,#2136,.F.);
#2931=ORIENTED_EDGE('',*,*,#2137,.F.);
#2932=ORIENTED_EDGE('',*,*,#2138,.T.);
#2933=ORIENTED_EDGE('',*,*,#2139,.F.);
#2934=ORIENTED_EDGE('',*,*,#2138,.F.);
#2935=ORIENTED_EDGE('',*,*,#2140,.F.);
#2936=ORIENTED_EDGE('',*,*,#2141,.F.);
#2937=ORIENTED_EDGE('',*,*,#2142,.F.);
#2938=ORIENTED_EDGE('',*,*,#2143,.F.);
#2939=ORIENTED_EDGE('',*,*,#2144,.F.);
#2940=ORIENTED_EDGE('',*,*,#2145,.T.);
#2941=ORIENTED_EDGE('',*,*,#2146,.F.);
#2942=ORIENTED_EDGE('',*,*,#2147,.F.);
#2943=ORIENTED_EDGE('',*,*,#2148,.F.);
#2944=ORIENTED_EDGE('',*,*,#2149,.F.);
#2945=ORIENTED_EDGE('',*,*,#2150,.F.);
#2946=ORIENTED_EDGE('',*,*,#2151,.F.);
#2947=ORIENTED_EDGE('',*,*,#2145,.F.);
#2948=ORIENTED_EDGE('',*,*,#2141,.T.);
#2949=ORIENTED_EDGE('',*,*,#2152,.T.);
#2950=ORIENTED_EDGE('',*,*,#2150,.T.);
#2951=ORIENTED_EDGE('',*,*,#2153,.F.);
#2952=ORIENTED_EDGE('',*,*,#2140,.T.);
#2953=ORIENTED_EDGE('',*,*,#2154,.T.);
#2954=ORIENTED_EDGE('',*,*,#2151,.T.);
#2955=ORIENTED_EDGE('',*,*,#2152,.F.);
#2956=ORIENTED_EDGE('',*,*,#2137,.T.);
#2957=ORIENTED_EDGE('',*,*,#2155,.T.);
#2958=ORIENTED_EDGE('',*,*,#2146,.T.);
#2959=ORIENTED_EDGE('',*,*,#2154,.F.);
#2960=ORIENTED_EDGE('',*,*,#2156,.F.);
#2961=ORIENTED_EDGE('',*,*,#2157,.T.);
#2962=ORIENTED_EDGE('',*,*,#2158,.T.);
#2963=ORIENTED_EDGE('',*,*,#2157,.F.);
#2964=ORIENTED_EDGE('',*,*,#2136,.T.);
#2965=ORIENTED_EDGE('',*,*,#2159,.T.);
#2966=ORIENTED_EDGE('',*,*,#2147,.T.);
#2967=ORIENTED_EDGE('',*,*,#2155,.F.);
#2968=ORIENTED_EDGE('',*,*,#2142,.T.);
#2969=ORIENTED_EDGE('',*,*,#2153,.T.);
#2970=ORIENTED_EDGE('',*,*,#2149,.T.);
#2971=ORIENTED_EDGE('',*,*,#2160,.F.);
#2972=ORIENTED_EDGE('',*,*,#2143,.T.);
#2973=ORIENTED_EDGE('',*,*,#2160,.T.);
#2974=ORIENTED_EDGE('',*,*,#2148,.T.);
#2975=ORIENTED_EDGE('',*,*,#2159,.F.);
#2976=ORIENTED_EDGE('',*,*,#2144,.T.);
#2977=ORIENTED_EDGE('',*,*,#2156,.T.);
#2978=ORIENTED_EDGE('',*,*,#2139,.T.);
#2979=ORIENTED_EDGE('',*,*,#2158,.F.);
#2980=ORIENTED_EDGE('',*,*,#2161,.F.);
#2981=ORIENTED_EDGE('',*,*,#2162,.F.);
#2982=ORIENTED_EDGE('',*,*,#2163,.F.);
#2983=ORIENTED_EDGE('',*,*,#2164,.F.);
#2984=ORIENTED_EDGE('',*,*,#2165,.F.);
#2985=ORIENTED_EDGE('',*,*,#2166,.F.);
#2986=ORIENTED_EDGE('',*,*,#2167,.F.);
#2987=ORIENTED_EDGE('',*,*,#2168,.F.);
#2988=ORIENTED_EDGE('',*,*,#2169,.F.);
#2989=ORIENTED_EDGE('',*,*,#2170,.F.);
#2990=ORIENTED_EDGE('',*,*,#2171,.F.);
#2991=ORIENTED_EDGE('',*,*,#2172,.F.);
#2992=ORIENTED_EDGE('',*,*,#2173,.F.);
#2993=ORIENTED_EDGE('',*,*,#2174,.F.);
#2994=ORIENTED_EDGE('',*,*,#2175,.F.);
#2995=ORIENTED_EDGE('',*,*,#2176,.F.);
#2996=ORIENTED_EDGE('',*,*,#2177,.F.);
#2997=ORIENTED_EDGE('',*,*,#2178,.F.);
#2998=ORIENTED_EDGE('',*,*,#2179,.F.);
#2999=ORIENTED_EDGE('',*,*,#2180,.F.);
#3000=ORIENTED_EDGE('',*,*,#2181,.F.);
#3001=ORIENTED_EDGE('',*,*,#2182,.F.);
#3002=ORIENTED_EDGE('',*,*,#2183,.F.);
#3003=ORIENTED_EDGE('',*,*,#2184,.F.);
#3004=ORIENTED_EDGE('',*,*,#2162,.T.);
#3005=ORIENTED_EDGE('',*,*,#2185,.T.);
#3006=ORIENTED_EDGE('',*,*,#2182,.T.);
#3007=ORIENTED_EDGE('',*,*,#2186,.T.);
#3008=ORIENTED_EDGE('',*,*,#2168,.T.);
#3009=ORIENTED_EDGE('',*,*,#2187,.T.);
#3010=ORIENTED_EDGE('',*,*,#2170,.T.);
#3011=ORIENTED_EDGE('',*,*,#2188,.T.);
#3012=ORIENTED_EDGE('',*,*,#2174,.T.);
#3013=ORIENTED_EDGE('',*,*,#2189,.T.);
#3014=ORIENTED_EDGE('',*,*,#2178,.T.);
#3015=ORIENTED_EDGE('',*,*,#2190,.T.);
#3016=ORIENTED_EDGE('',*,*,#2191,.T.);
#3017=ORIENTED_EDGE('',*,*,#2173,.T.);
#3018=ORIENTED_EDGE('',*,*,#2192,.T.);
#3019=ORIENTED_EDGE('',*,*,#2179,.T.);
#3020=ORIENTED_EDGE('',*,*,#2189,.F.);
#3021=ORIENTED_EDGE('',*,*,#2169,.T.);
#3022=ORIENTED_EDGE('',*,*,#2193,.T.);
#3023=ORIENTED_EDGE('',*,*,#2175,.T.);
#3024=ORIENTED_EDGE('',*,*,#2188,.F.);
#3025=ORIENTED_EDGE('',*,*,#2165,.T.);
#3026=ORIENTED_EDGE('',*,*,#2186,.F.);
#3027=ORIENTED_EDGE('',*,*,#2181,.T.);
#3028=ORIENTED_EDGE('',*,*,#2194,.T.);
#3029=ORIENTED_EDGE('',*,*,#2167,.T.);
#3030=ORIENTED_EDGE('',*,*,#2195,.T.);
#3031=ORIENTED_EDGE('',*,*,#2171,.T.);
#3032=ORIENTED_EDGE('',*,*,#2187,.F.);
#3033=ORIENTED_EDGE('',*,*,#2161,.T.);
#3034=ORIENTED_EDGE('',*,*,#2196,.T.);
#3035=ORIENTED_EDGE('',*,*,#2183,.T.);
#3036=ORIENTED_EDGE('',*,*,#2185,.F.);
#3037=ORIENTED_EDGE('',*,*,#2163,.T.);
#3038=ORIENTED_EDGE('',*,*,#2190,.F.);
#3039=ORIENTED_EDGE('',*,*,#2177,.T.);
#3040=ORIENTED_EDGE('',*,*,#2197,.T.);
#3041=ORIENTED_EDGE('',*,*,#2198,.F.);
#3042=ORIENTED_EDGE('',*,*,#2199,.T.);
#3043=ORIENTED_EDGE('',*,*,#2200,.T.);
#3044=ORIENTED_EDGE('',*,*,#2201,.F.);
#3045=ORIENTED_EDGE('',*,*,#2202,.F.);
#3046=ORIENTED_EDGE('',*,*,#2201,.T.);
#3047=ORIENTED_EDGE('',*,*,#2203,.T.);
#3048=ORIENTED_EDGE('',*,*,#2204,.F.);
#3049=ORIENTED_EDGE('',*,*,#2205,.F.);
#3050=ORIENTED_EDGE('',*,*,#2204,.T.);
#3051=ORIENTED_EDGE('',*,*,#2206,.T.);
#3052=ORIENTED_EDGE('',*,*,#2207,.F.);
#3053=ORIENTED_EDGE('',*,*,#2208,.F.);
#3054=ORIENTED_EDGE('',*,*,#2207,.T.);
#3055=ORIENTED_EDGE('',*,*,#2209,.T.);
#3056=ORIENTED_EDGE('',*,*,#2210,.F.);
#3057=ORIENTED_EDGE('',*,*,#2211,.F.);
#3058=ORIENTED_EDGE('',*,*,#2212,.T.);
#3059=ORIENTED_EDGE('',*,*,#2213,.T.);
#3060=ORIENTED_EDGE('',*,*,#2199,.F.);
#3061=ORIENTED_EDGE('',*,*,#2214,.F.);
#3062=ORIENTED_EDGE('',*,*,#2210,.T.);
#3063=ORIENTED_EDGE('',*,*,#2215,.T.);
#3064=ORIENTED_EDGE('',*,*,#2212,.F.);
#3065=ORIENTED_EDGE('',*,*,#2215,.F.);
#3066=ORIENTED_EDGE('',*,*,#2209,.F.);
#3067=ORIENTED_EDGE('',*,*,#2206,.F.);
#3068=ORIENTED_EDGE('',*,*,#2203,.F.);
#3069=ORIENTED_EDGE('',*,*,#2200,.F.);
#3070=ORIENTED_EDGE('',*,*,#2213,.F.);
#3071=ORIENTED_EDGE('',*,*,#2216,.F.);
#3072=ORIENTED_EDGE('',*,*,#2191,.F.);
#3073=ORIENTED_EDGE('',*,*,#2217,.T.);
#3074=ORIENTED_EDGE('',*,*,#2216,.T.);
#3075=ORIENTED_EDGE('',*,*,#2217,.F.);
#3076=ORIENTED_EDGE('',*,*,#2164,.T.);
#3077=ORIENTED_EDGE('',*,*,#2197,.F.);
#3078=ORIENTED_EDGE('',*,*,#2180,.T.);
#3079=ORIENTED_EDGE('',*,*,#2192,.F.);
#3080=ORIENTED_EDGE('',*,*,#2176,.T.);
#3081=ORIENTED_EDGE('',*,*,#2193,.F.);
#3082=ORIENTED_EDGE('',*,*,#2172,.T.);
#3083=ORIENTED_EDGE('',*,*,#2195,.F.);
#3084=ORIENTED_EDGE('',*,*,#2166,.T.);
#3085=ORIENTED_EDGE('',*,*,#2194,.F.);
#3086=ORIENTED_EDGE('',*,*,#2184,.T.);
#3087=ORIENTED_EDGE('',*,*,#2196,.F.);
#3088=ORIENTED_EDGE('',*,*,#2208,.T.);
#3089=ORIENTED_EDGE('',*,*,#2214,.T.);
#3090=ORIENTED_EDGE('',*,*,#2211,.T.);
#3091=ORIENTED_EDGE('',*,*,#2198,.T.);
#3092=ORIENTED_EDGE('',*,*,#2202,.T.);
#3093=ORIENTED_EDGE('',*,*,#2205,.T.);
#3094=CYLINDRICAL_SURFACE('',#3471,0.800000000000001);
#3095=CYLINDRICAL_SURFACE('',#3476,0.8);
#3096=CYLINDRICAL_SURFACE('',#3481,0.275);
#3097=CYLINDRICAL_SURFACE('',#3483,0.275);
#3098=CYLINDRICAL_SURFACE('',#3485,0.425);
#3099=CYLINDRICAL_SURFACE('',#3488,1.3);
#3100=CYLINDRICAL_SURFACE('',#3510,0.2117);
#3101=CYLINDRICAL_SURFACE('',#3523,0.265);
#3102=CYLINDRICAL_SURFACE('',#3527,0.5);
#3103=CYLINDRICAL_SURFACE('',#3534,0.25);
#3104=CYLINDRICAL_SURFACE('',#3541,0.425);
#3105=CYLINDRICAL_SURFACE('',#3549,0.24505);
#3106=CYLINDRICAL_SURFACE('',#3595,0.21);
#3107=CYLINDRICAL_SURFACE('',#3609,0.3933);
#3108=CYLINDRICAL_SURFACE('',#3627,0.164999999999999);
#3109=CYLINDRICAL_SURFACE('',#3630,0.164999999999999);
#3110=CYLINDRICAL_SURFACE('',#3642,1.8);
#3111=CYLINDRICAL_SURFACE('',#3644,0.425);
#3112=CYLINDRICAL_SURFACE('',#3648,0.4);
#3113=CYLINDRICAL_SURFACE('',#3653,0.4);
#3114=CYLINDRICAL_SURFACE('',#3658,0.225);
#3115=CYLINDRICAL_SURFACE('',#3660,0.225);
#3116=CYLINDRICAL_SURFACE('',#3673,0.35);
#3117=CYLINDRICAL_SURFACE('',#3681,0.1954);
#3118=CYLINDRICAL_SURFACE('',#3695,0.42);
#3119=CYLINDRICAL_SURFACE('',#3698,0.8);
#3120=CYLINDRICAL_SURFACE('',#3721,0.338975);
#3121=CYLINDRICAL_SURFACE('',#3730,0.4);
#3122=CYLINDRICAL_SURFACE('',#3733,0.4);
#3123=CYLINDRICAL_SURFACE('',#3736,0.4);
#3124=CYLINDRICAL_SURFACE('',#3739,0.4);
#3125=CYLINDRICAL_SURFACE('',#3742,0.4);
#3126=CYLINDRICAL_SURFACE('',#3745,0.4);
#3127=CYLINDRICAL_SURFACE('',#3756,1.8);
#3128=CYLINDRICAL_SURFACE('',#3758,1.8);
#3129=CYLINDRICAL_SURFACE('',#3760,1.8);
#3130=CYLINDRICAL_SURFACE('',#3762,1.8);
#3131=CYLINDRICAL_SURFACE('',#3764,1.8);
#3132=CYLINDRICAL_SURFACE('',#3766,1.8);
#3133=CYLINDRICAL_SURFACE('',#3776,0.425);
#3134=ADVANCED_FACE('',(#341),#3094,.T.);
#3135=ADVANCED_FACE('',(#342,#169),#206,.F.);
#3136=ADVANCED_FACE('',(#343),#3095,.T.);
#3137=ADVANCED_FACE('',(#344,#170),#207,.F.);
#3138=ADVANCED_FACE('',(#345),#3096,.F.);
#3139=ADVANCED_FACE('',(#346),#3097,.F.);
#3140=ADVANCED_FACE('',(#347),#3098,.F.);
#3141=ADVANCED_FACE('',(#348),#3099,.T.);
#3142=ADVANCED_FACE('',(#349,#171),#208,.T.);
#3143=ADVANCED_FACE('',(#350),#209,.T.);
#3144=ADVANCED_FACE('',(#351),#210,.T.);
#3145=ADVANCED_FACE('',(#352),#211,.T.);
#3146=ADVANCED_FACE('',(#353),#212,.T.);
#3147=ADVANCED_FACE('',(#354,#172,#173,#174),#213,.T.);
#3148=ADVANCED_FACE('',(#355,#175,#176,#177),#214,.F.);
#3149=ADVANCED_FACE('',(#356),#215,.F.);
#3150=ADVANCED_FACE('',(#357),#216,.T.);
#3151=ADVANCED_FACE('',(#358,#178),#217,.T.);
#3152=ADVANCED_FACE('',(#359),#218,.T.);
#3153=ADVANCED_FACE('',(#360),#219,.T.);
#3154=ADVANCED_FACE('',(#361),#220,.F.);
#3155=ADVANCED_FACE('',(#362),#221,.T.);
#3156=ADVANCED_FACE('',(#363),#222,.T.);
#3157=ADVANCED_FACE('',(#364),#223,.T.);
#3158=ADVANCED_FACE('',(#365),#3100,.F.);
#3159=ADVANCED_FACE('',(#366),#224,.F.);
#3160=ADVANCED_FACE('',(#367),#225,.F.);
#3161=ADVANCED_FACE('',(#368),#226,.T.);
#3162=ADVANCED_FACE('',(#369),#227,.T.);
#3163=ADVANCED_FACE('',(#370),#109,.F.);
#3164=ADVANCED_FACE('',(#371),#3101,.F.);
#3165=ADVANCED_FACE('',(#372,#179),#228,.T.);
#3166=ADVANCED_FACE('',(#373),#3102,.T.);
#3167=ADVANCED_FACE('',(#374,#180),#229,.F.);
#3168=ADVANCED_FACE('',(#375,#181),#230,.T.);
#3169=ADVANCED_FACE('',(#376),#3103,.T.);
#3170=ADVANCED_FACE('',(#377),#231,.F.);
#3171=ADVANCED_FACE('',(#378),#232,.T.);
#3172=ADVANCED_FACE('',(#379),#110,.T.);
#3173=ADVANCED_FACE('',(#380),#3104,.T.);
#3174=ADVANCED_FACE('',(#381),#111,.T.);
#3175=ADVANCED_FACE('',(#382,#182),#233,.T.);
#3176=ADVANCED_FACE('',(#383),#112,.T.);
#3177=ADVANCED_FACE('',(#384),#3105,.T.);
#3178=ADVANCED_FACE('',(#385),#234,.F.);
#3179=ADVANCED_FACE('',(#386),#235,.F.);
#3180=ADVANCED_FACE('',(#387),#236,.F.);
#3181=ADVANCED_FACE('',(#388),#237,.F.);
#3182=ADVANCED_FACE('',(#389),#238,.F.);
#3183=ADVANCED_FACE('',(#390),#239,.F.);
#3184=ADVANCED_FACE('',(#391),#240,.F.);
#3185=ADVANCED_FACE('',(#392),#241,.F.);
#3186=ADVANCED_FACE('',(#393),#242,.F.);
#3187=ADVANCED_FACE('',(#394),#243,.F.);
#3188=ADVANCED_FACE('',(#395),#244,.F.);
#3189=ADVANCED_FACE('',(#396),#245,.F.);
#3190=ADVANCED_FACE('',(#397),#246,.F.);
#3191=ADVANCED_FACE('',(#398),#247,.F.);
#3192=ADVANCED_FACE('',(#399),#248,.F.);
#3193=ADVANCED_FACE('',(#400),#249,.F.);
#3194=ADVANCED_FACE('',(#401),#250,.F.);
#3195=ADVANCED_FACE('',(#402),#251,.F.);
#3196=ADVANCED_FACE('',(#403),#252,.F.);
#3197=ADVANCED_FACE('',(#404),#253,.F.);
#3198=ADVANCED_FACE('',(#405),#254,.F.);
#3199=ADVANCED_FACE('',(#406),#255,.F.);
#3200=ADVANCED_FACE('',(#407),#256,.F.);
#3201=ADVANCED_FACE('',(#408),#257,.F.);
#3202=ADVANCED_FACE('',(#409),#258,.F.);
#3203=ADVANCED_FACE('',(#410),#259,.F.);
#3204=ADVANCED_FACE('',(#411),#260,.F.);
#3205=ADVANCED_FACE('',(#412),#261,.F.);
#3206=ADVANCED_FACE('',(#413),#262,.F.);
#3207=ADVANCED_FACE('',(#414),#263,.F.);
#3208=ADVANCED_FACE('',(#415),#264,.F.);
#3209=ADVANCED_FACE('',(#416),#265,.F.);
#3210=ADVANCED_FACE('',(#417),#266,.F.);
#3211=ADVANCED_FACE('',(#418),#267,.F.);
#3212=ADVANCED_FACE('',(#419),#268,.F.);
#3213=ADVANCED_FACE('',(#420),#269,.F.);
#3214=ADVANCED_FACE('',(#421),#270,.F.);
#3215=ADVANCED_FACE('',(#422),#271,.F.);
#3216=ADVANCED_FACE('',(#423),#272,.F.);
#3217=ADVANCED_FACE('',(#424),#273,.F.);
#3218=ADVANCED_FACE('',(#425),#274,.F.);
#3219=ADVANCED_FACE('',(#426),#275,.F.);
#3220=ADVANCED_FACE('',(#427),#276,.F.);
#3221=ADVANCED_FACE('',(#428),#277,.F.);
#3222=ADVANCED_FACE('',(#429),#3106,.F.);
#3223=ADVANCED_FACE('',(#430),#278,.T.);
#3224=ADVANCED_FACE('',(#431),#279,.T.);
#3225=ADVANCED_FACE('',(#432),#280,.T.);
#3226=ADVANCED_FACE('',(#433),#281,.T.);
#3227=ADVANCED_FACE('',(#434),#282,.T.);
#3228=ADVANCED_FACE('',(#435),#283,.T.);
#3229=ADVANCED_FACE('',(#436),#284,.T.);
#3230=ADVANCED_FACE('',(#437),#285,.T.);
#3231=ADVANCED_FACE('',(#438,#183),#286,.T.);
#3232=ADVANCED_FACE('',(#439,#184),#287,.F.);
#3233=ADVANCED_FACE('',(#440),#3107,.T.);
#3234=ADVANCED_FACE('',(#441),#113,.T.);
#3235=ADVANCED_FACE('',(#442),#288,.T.);
#3236=ADVANCED_FACE('',(#443),#114,.T.);
#3237=ADVANCED_FACE('',(#444),#289,.T.);
#3238=ADVANCED_FACE('',(#445),#290,.T.);
#3239=ADVANCED_FACE('',(#446),#291,.T.);
#3240=ADVANCED_FACE('',(#447),#292,.T.);
#3241=ADVANCED_FACE('',(#448),#293,.T.);
#3242=ADVANCED_FACE('',(#449),#294,.T.);
#3243=ADVANCED_FACE('',(#450),#295,.T.);
#3244=ADVANCED_FACE('',(#451,#185),#296,.F.);
#3245=ADVANCED_FACE('',(#452),#3108,.F.);
#3246=ADVANCED_FACE('',(#453),#3109,.F.);
#3247=ADVANCED_FACE('',(#454,#186,#187,#188),#297,.T.);
#3248=ADVANCED_FACE('',(#455),#298,.T.);
#3249=ADVANCED_FACE('',(#456),#299,.T.);
#3250=ADVANCED_FACE('',(#457),#300,.T.);
#3251=ADVANCED_FACE('',(#458,#189,#190),#301,.F.);
#3252=ADVANCED_FACE('',(#459),#3110,.T.);
#3253=ADVANCED_FACE('',(#460),#3111,.F.);
#3254=ADVANCED_FACE('',(#461,#191),#302,.F.);
#3255=ADVANCED_FACE('',(#462),#3112,.F.);
#3256=ADVANCED_FACE('',(#463,#192),#303,.T.);
#3257=ADVANCED_FACE('',(#464),#3113,.F.);
#3258=ADVANCED_FACE('',(#465,#193),#304,.T.);
#3259=ADVANCED_FACE('',(#466),#3114,.F.);
#3260=ADVANCED_FACE('',(#467),#3115,.F.);
#3261=ADVANCED_FACE('',(#468),#305,.T.);
#3262=ADVANCED_FACE('',(#469),#306,.T.);
#3263=ADVANCED_FACE('',(#470),#307,.T.);
#3264=ADVANCED_FACE('',(#471),#308,.T.);
#3265=ADVANCED_FACE('',(#472,#194,#195),#309,.T.);
#3266=ADVANCED_FACE('',(#473,#196,#197),#310,.F.);
#3267=ADVANCED_FACE('',(#474),#311,.T.);
#3268=ADVANCED_FACE('',(#475),#115,.T.);
#3269=ADVANCED_FACE('',(#476),#3116,.T.);
#3270=ADVANCED_FACE('',(#477),#116,.T.);
#3271=ADVANCED_FACE('',(#478,#198),#312,.T.);
#3272=ADVANCED_FACE('',(#479),#117,.T.);
#3273=ADVANCED_FACE('',(#480),#3117,.T.);
#3274=ADVANCED_FACE('',(#481),#118,.T.);
#3275=ADVANCED_FACE('',(#482),#313,.T.);
#3276=ADVANCED_FACE('',(#483),#314,.F.);
#3277=ADVANCED_FACE('',(#484),#315,.F.);
#3278=ADVANCED_FACE('',(#485),#316,.F.);
#3279=ADVANCED_FACE('',(#486),#317,.F.);
#3280=ADVANCED_FACE('',(#487),#318,.F.);
#3281=ADVANCED_FACE('',(#488),#319,.F.);
#3282=ADVANCED_FACE('',(#489),#320,.F.);
#3283=ADVANCED_FACE('',(#490),#321,.F.);
#3284=ADVANCED_FACE('',(#491),#3118,.F.);
#3285=ADVANCED_FACE('',(#492),#3119,.T.);
#3286=ADVANCED_FACE('',(#493,#199),#322,.T.);
#3287=ADVANCED_FACE('',(#494,#200),#323,.F.);
#3288=ADVANCED_FACE('',(#495),#119,.T.);
#3289=ADVANCED_FACE('',(#496),#120,.T.);
#3290=ADVANCED_FACE('',(#497),#324,.T.);
#3291=ADVANCED_FACE('',(#498),#325,.T.);
#3292=ADVANCED_FACE('',(#499),#326,.T.);
#3293=ADVANCED_FACE('',(#500),#3120,.F.);
#3294=ADVANCED_FACE('',(#501),#327,.T.);
#3295=ADVANCED_FACE('',(#502),#328,.T.);
#3296=ADVANCED_FACE('',(#503),#329,.T.);
#3297=ADVANCED_FACE('',(#504,#201),#330,.T.);
#3298=ADVANCED_FACE('',(#505,#202),#331,.F.);
#3299=ADVANCED_FACE('',(#506),#3121,.F.);
#3300=ADVANCED_FACE('',(#507),#3122,.F.);
#3301=ADVANCED_FACE('',(#508),#3123,.F.);
#3302=ADVANCED_FACE('',(#509),#3124,.F.);
#3303=ADVANCED_FACE('',(#510),#3125,.F.);
#3304=ADVANCED_FACE('',(#511),#3126,.F.);
#3305=ADVANCED_FACE('',(#512,#203),#332,.T.);
#3306=ADVANCED_FACE('',(#513),#3127,.T.);
#3307=ADVANCED_FACE('',(#514),#3128,.T.);
#3308=ADVANCED_FACE('',(#515),#3129,.T.);
#3309=ADVANCED_FACE('',(#516),#3130,.T.);
#3310=ADVANCED_FACE('',(#517),#3131,.T.);
#3311=ADVANCED_FACE('',(#518),#3132,.T.);
#3312=ADVANCED_FACE('',(#519),#333,.F.);
#3313=ADVANCED_FACE('',(#520),#334,.F.);
#3314=ADVANCED_FACE('',(#521),#335,.F.);
#3315=ADVANCED_FACE('',(#522),#336,.F.);
#3316=ADVANCED_FACE('',(#523),#337,.F.);
#3317=ADVANCED_FACE('',(#524),#338,.F.);
#3318=ADVANCED_FACE('',(#525,#204),#339,.F.);
#3319=ADVANCED_FACE('',(#526),#3133,.F.);
#3320=ADVANCED_FACE('',(#527,#205),#340,.F.);
#3321=CLOSED_SHELL('',(#3134,#3135,#3136,#3137,#3138,#3139,#3140,#3141,
#3142,#3143,#3144,#3145,#3146,#3147,#3148));
#3322=CLOSED_SHELL('',(#3149,#3150,#3151,#3152,#3153,#3154,#3155,#3156,
#3157,#3158,#3159,#3160,#3161,#3162));
#3323=CLOSED_SHELL('',(#3163,#3164,#3165,#3166,#3167));
#3324=CLOSED_SHELL('',(#3168,#3169,#3170,#3171,#3172,#3173,#3174,#3175,
#3176,#3177));
#3325=CLOSED_SHELL('',(#3178,#3179,#3180,#3181,#3182,#3183,#3184,#3185));
#3326=CLOSED_SHELL('',(#3186,#3187,#3188,#3189,#3190,#3191,#3192,#3193,
#3194,#3195,#3196,#3197,#3198,#3199,#3200,#3201,#3202,#3203,#3204,#3205,
#3206,#3207,#3208,#3209,#3210,#3211,#3212,#3213,#3214,#3215,#3216,#3217,
#3218,#3219,#3220,#3221,#3222,#3223,#3224,#3225,#3226,#3227,#3228,#3229,
#3230,#3231,#3232));
#3327=CLOSED_SHELL('',(#3233,#3234,#3235,#3236,#3237,#3238,#3239,#3240,
#3241,#3242,#3243,#3244));
#3328=CLOSED_SHELL('',(#3245,#3246,#3247,#3248,#3249,#3250,#3251,#3252,
#3253,#3254));
#3329=CLOSED_SHELL('',(#3255,#3256,#3257,#3258,#3259,#3260,#3261,#3262,
#3263,#3264,#3265,#3266));
#3330=CLOSED_SHELL('',(#3267,#3268,#3269,#3270,#3271,#3272,#3273,#3274,
#3275));
#3331=CLOSED_SHELL('',(#3276,#3277,#3278,#3279,#3280,#3281,#3282,#3283));
#3332=CLOSED_SHELL('',(#3284,#3285,#3286,#3287));
#3333=CLOSED_SHELL('',(#3288,#3289,#3290,#3291,#3292,#3293,#3294,#3295,
#3296,#3297,#3298));
#3334=CLOSED_SHELL('',(#3299,#3300,#3301,#3302,#3303,#3304,#3305,#3306,
#3307,#3308,#3309,#3310,#3311,#3312,#3313,#3314,#3315,#3316,#3317,#3318,
#3319,#3320));
#3335=DERIVED_UNIT_ELEMENT(#3359,1.);
#3336=DERIVED_UNIT_ELEMENT(#5763,-3.);
#3337=DERIVED_UNIT_ELEMENT(#3359,1.);
#3338=DERIVED_UNIT_ELEMENT(#5763,-3.);
#3339=DERIVED_UNIT_ELEMENT(#3359,1.);
#3340=DERIVED_UNIT_ELEMENT(#5763,-3.);
#3341=DERIVED_UNIT_ELEMENT(#3359,1.);
#3342=DERIVED_UNIT_ELEMENT(#5763,-3.);
#3343=DERIVED_UNIT_ELEMENT(#3359,1.);
#3344=DERIVED_UNIT_ELEMENT(#5763,-3.);
#3345=DERIVED_UNIT_ELEMENT(#3359,1.);
#3346=DERIVED_UNIT_ELEMENT(#5763,-3.);
#3347=DERIVED_UNIT_ELEMENT(#3359,1.);
#3348=DERIVED_UNIT_ELEMENT(#5763,-3.);
#3349=DERIVED_UNIT_ELEMENT(#3359,1.);
#3350=DERIVED_UNIT_ELEMENT(#5763,-3.);
#3351=DERIVED_UNIT_ELEMENT(#3359,1.);
#3352=DERIVED_UNIT_ELEMENT(#5763,-3.);
#3353=DERIVED_UNIT_ELEMENT(#3359,1.);
#3354=DERIVED_UNIT_ELEMENT(#5763,-3.);
#3355=DERIVED_UNIT_ELEMENT(#3359,1.);
#3356=DERIVED_UNIT_ELEMENT(#5763,-3.);
#3357=DERIVED_UNIT_ELEMENT(#3359,1.);
#3358=DERIVED_UNIT_ELEMENT(#5763,-3.);
#3359=(
MASS_UNIT()
NAMED_UNIT(*)
SI_UNIT(.KILO.,.GRAM.)
);
#3360=DERIVED_UNIT((#3335,#3336));
#3361=DERIVED_UNIT((#3337,#3338));
#3362=DERIVED_UNIT((#3339,#3340));
#3363=DERIVED_UNIT((#3341,#3342));
#3364=DERIVED_UNIT((#3343,#3344));
#3365=DERIVED_UNIT((#3345,#3346));
#3366=DERIVED_UNIT((#3347,#3348));
#3367=DERIVED_UNIT((#3349,#3350));
#3368=DERIVED_UNIT((#3351,#3352));
#3369=DERIVED_UNIT((#3353,#3354));
#3370=DERIVED_UNIT((#3355,#3356));
#3371=DERIVED_UNIT((#3357,#3358));
#3372=MEASURE_REPRESENTATION_ITEM('density measure',
POSITIVE_RATIO_MEASURE(7850.),#3360);
#3373=MEASURE_REPRESENTATION_ITEM('density measure',
POSITIVE_RATIO_MEASURE(7850.),#3361);
#3374=MEASURE_REPRESENTATION_ITEM('density measure',
POSITIVE_RATIO_MEASURE(7850.),#3362);
#3375=MEASURE_REPRESENTATION_ITEM('density measure',
POSITIVE_RATIO_MEASURE(7850.),#3363);
#3376=MEASURE_REPRESENTATION_ITEM('density measure',
POSITIVE_RATIO_MEASURE(7850.),#3364);
#3377=MEASURE_REPRESENTATION_ITEM('density measure',
POSITIVE_RATIO_MEASURE(7850.),#3365);
#3378=MEASURE_REPRESENTATION_ITEM('density measure',
POSITIVE_RATIO_MEASURE(7850.),#3366);
#3379=MEASURE_REPRESENTATION_ITEM('density measure',
POSITIVE_RATIO_MEASURE(7850.),#3367);
#3380=MEASURE_REPRESENTATION_ITEM('density measure',
POSITIVE_RATIO_MEASURE(7850.),#3368);
#3381=MEASURE_REPRESENTATION_ITEM('density measure',
POSITIVE_RATIO_MEASURE(7850.),#3369);
#3382=MEASURE_REPRESENTATION_ITEM('density measure',
POSITIVE_RATIO_MEASURE(7850.),#3370);
#3383=MEASURE_REPRESENTATION_ITEM('density measure',
POSITIVE_RATIO_MEASURE(7850.),#3371);
#3384=PROPERTY_DEFINITION_REPRESENTATION(#3444,#3408);
#3385=PROPERTY_DEFINITION_REPRESENTATION(#3445,#3409);
#3386=PROPERTY_DEFINITION_REPRESENTATION(#3446,#3410);
#3387=PROPERTY_DEFINITION_REPRESENTATION(#3447,#3411);
#3388=PROPERTY_DEFINITION_REPRESENTATION(#3448,#3412);
#3389=PROPERTY_DEFINITION_REPRESENTATION(#3449,#3413);
#3390=PROPERTY_DEFINITION_REPRESENTATION(#3450,#3414);
#3391=PROPERTY_DEFINITION_REPRESENTATION(#3451,#3415);
#3392=PROPERTY_DEFINITION_REPRESENTATION(#3452,#3416);
#3393=PROPERTY_DEFINITION_REPRESENTATION(#3453,#3417);
#3394=PROPERTY_DEFINITION_REPRESENTATION(#3454,#3418);
#3395=PROPERTY_DEFINITION_REPRESENTATION(#3455,#3419);
#3396=PROPERTY_DEFINITION_REPRESENTATION(#3456,#3420);
#3397=PROPERTY_DEFINITION_REPRESENTATION(#3457,#3421);
#3398=PROPERTY_DEFINITION_REPRESENTATION(#3458,#3422);
#3399=PROPERTY_DEFINITION_REPRESENTATION(#3459,#3423);
#3400=PROPERTY_DEFINITION_REPRESENTATION(#3460,#3424);
#3401=PROPERTY_DEFINITION_REPRESENTATION(#3461,#3425);
#3402=PROPERTY_DEFINITION_REPRESENTATION(#3462,#3426);
#3403=PROPERTY_DEFINITION_REPRESENTATION(#3463,#3427);
#3404=PROPERTY_DEFINITION_REPRESENTATION(#3464,#3428);
#3405=PROPERTY_DEFINITION_REPRESENTATION(#3465,#3429);
#3406=PROPERTY_DEFINITION_REPRESENTATION(#3466,#3430);
#3407=PROPERTY_DEFINITION_REPRESENTATION(#3467,#3431);
#3408=REPRESENTATION('material name',(#3432),#5748);
#3409=REPRESENTATION('density',(#3372),#5748);
#3410=REPRESENTATION('material name',(#3433),#5749);
#3411=REPRESENTATION('density',(#3373),#5749);
#3412=REPRESENTATION('material name',(#3434),#5750);
#3413=REPRESENTATION('density',(#3374),#5750);
#3414=REPRESENTATION('material name',(#3435),#5751);
#3415=REPRESENTATION('density',(#3375),#5751);
#3416=REPRESENTATION('material name',(#3436),#5752);
#3417=REPRESENTATION('density',(#3376),#5752);
#3418=REPRESENTATION('material name',(#3437),#5753);
#3419=REPRESENTATION('density',(#3377),#5753);
#3420=REPRESENTATION('material name',(#3438),#5755);
#3421=REPRESENTATION('density',(#3378),#5755);
#3422=REPRESENTATION('material name',(#3439),#5756);
#3423=REPRESENTATION('density',(#3379),#5756);
#3424=REPRESENTATION('material name',(#3440),#5757);
#3425=REPRESENTATION('density',(#3380),#5757);
#3426=REPRESENTATION('material name',(#3441),#5758);
#3427=REPRESENTATION('density',(#3381),#5758);
#3428=REPRESENTATION('material name',(#3442),#5759);
#3429=REPRESENTATION('density',(#3382),#5759);
#3430=REPRESENTATION('material name',(#3443),#5760);
#3431=REPRESENTATION('density',(#3383),#5760);
#3432=DESCRIPTIVE_REPRESENTATION_ITEM('Steel','Steel');
#3433=DESCRIPTIVE_REPRESENTATION_ITEM('Steel','Steel');
#3434=DESCRIPTIVE_REPRESENTATION_ITEM('Steel','Steel');
#3435=DESCRIPTIVE_REPRESENTATION_ITEM('Steel','Steel');
#3436=DESCRIPTIVE_REPRESENTATION_ITEM('Steel','Steel');
#3437=DESCRIPTIVE_REPRESENTATION_ITEM('Steel','Steel');
#3438=DESCRIPTIVE_REPRESENTATION_ITEM('Steel','Steel');
#3439=DESCRIPTIVE_REPRESENTATION_ITEM('Steel','Steel');
#3440=DESCRIPTIVE_REPRESENTATION_ITEM('Steel','Steel');
#3441=DESCRIPTIVE_REPRESENTATION_ITEM('Steel','Steel');
#3442=DESCRIPTIVE_REPRESENTATION_ITEM('Steel','Steel');
#3443=DESCRIPTIVE_REPRESENTATION_ITEM('Steel','Steel');
#3444=PROPERTY_DEFINITION('material property','material name',#5833);
#3445=PROPERTY_DEFINITION('material property','density of part',#5833);
#3446=PROPERTY_DEFINITION('material property','material name',#5834);
#3447=PROPERTY_DEFINITION('material property','density of part',#5834);
#3448=PROPERTY_DEFINITION('material property','material name',#5835);
#3449=PROPERTY_DEFINITION('material property','density of part',#5835);
#3450=PROPERTY_DEFINITION('material property','material name',#5836);
#3451=PROPERTY_DEFINITION('material property','density of part',#5836);
#3452=PROPERTY_DEFINITION('material property','material name',#5837);
#3453=PROPERTY_DEFINITION('material property','density of part',#5837);
#3454=PROPERTY_DEFINITION('material property','material name',#5838);
#3455=PROPERTY_DEFINITION('material property','density of part',#5838);
#3456=PROPERTY_DEFINITION('material property','material name',#5840);
#3457=PROPERTY_DEFINITION('material property','density of part',#5840);
#3458=PROPERTY_DEFINITION('material property','material name',#5841);
#3459=PROPERTY_DEFINITION('material property','density of part',#5841);
#3460=PROPERTY_DEFINITION('material property','material name',#5842);
#3461=PROPERTY_DEFINITION('material property','density of part',#5842);
#3462=PROPERTY_DEFINITION('material property','material name',#5843);
#3463=PROPERTY_DEFINITION('material property','density of part',#5843);
#3464=PROPERTY_DEFINITION('material property','material name',#5844);
#3465=PROPERTY_DEFINITION('material property','density of part',#5844);
#3466=PROPERTY_DEFINITION('material property','material name',#5845);
#3467=PROPERTY_DEFINITION('material property','density of part',#5845);
#3468=AXIS2_PLACEMENT_3D('',#4747,#3787,#3788);
#3469=AXIS2_PLACEMENT_3D('',#4748,#3789,#3790);
#3470=AXIS2_PLACEMENT_3D('',#4749,#3791,#3792);
#3471=AXIS2_PLACEMENT_3D('',#4750,#3793,#3794);
#3472=AXIS2_PLACEMENT_3D('',#4752,#3795,#3796);
#3473=AXIS2_PLACEMENT_3D('',#4755,#3798,#3799);
#3474=AXIS2_PLACEMENT_3D('',#4756,#3800,#3801);
#3475=AXIS2_PLACEMENT_3D('',#4758,#3802,#3803);
#3476=AXIS2_PLACEMENT_3D('',#4759,#3804,#3805);
#3477=AXIS2_PLACEMENT_3D('',#4761,#3806,#3807);
#3478=AXIS2_PLACEMENT_3D('',#4764,#3809,#3810);
#3479=AXIS2_PLACEMENT_3D('',#4765,#3811,#3812);
#3480=AXIS2_PLACEMENT_3D('',#4767,#3813,#3814);
#3481=AXIS2_PLACEMENT_3D('',#4768,#3815,#3816);
#3482=AXIS2_PLACEMENT_3D('',#4771,#3818,#3819);
#3483=AXIS2_PLACEMENT_3D('',#4772,#3820,#3821);
#3484=AXIS2_PLACEMENT_3D('',#4775,#3823,#3824);
#3485=AXIS2_PLACEMENT_3D('',#4776,#3825,#3826);
#3486=AXIS2_PLACEMENT_3D('',#4778,#3827,#3828);
#3487=AXIS2_PLACEMENT_3D('',#4781,#3830,#3831);
#3488=AXIS2_PLACEMENT_3D('',#4782,#3832,#3833);
#3489=AXIS2_PLACEMENT_3D('',#4784,#3834,#3835);
#3490=AXIS2_PLACEMENT_3D('',#4787,#3837,#3838);
#3491=AXIS2_PLACEMENT_3D('',#4788,#3839,#3840);
#3492=AXIS2_PLACEMENT_3D('',#4789,#3841,#3842);
#3493=AXIS2_PLACEMENT_3D('',#4798,#3847,#3848);
#3494=AXIS2_PLACEMENT_3D('',#4804,#3852,#3853);
#3495=AXIS2_PLACEMENT_3D('',#4810,#3857,#3858);
#3496=AXIS2_PLACEMENT_3D('',#4813,#3861,#3862);
#3497=AXIS2_PLACEMENT_3D('',#4814,#3863,#3864);
#3498=AXIS2_PLACEMENT_3D('',#4815,#3865,#3866);
#3499=AXIS2_PLACEMENT_3D('',#4816,#3867,#3868);
#3500=AXIS2_PLACEMENT_3D('',#4825,#3873,#3874);
#3501=AXIS2_PLACEMENT_3D('',#4831,#3878,#3879);
#3502=AXIS2_PLACEMENT_3D('',#4838,#3883,#3884);
#3503=AXIS2_PLACEMENT_3D('',#4839,#3885,#3886);
#3504=AXIS2_PLACEMENT_3D('',#4853,#3894,#3895);
#3505=AXIS2_PLACEMENT_3D('',#4857,#3898,#3899);
#3506=AXIS2_PLACEMENT_3D('',#4861,#3902,#3903);
#3507=AXIS2_PLACEMENT_3D('',#4871,#3909,#3910);
#3508=AXIS2_PLACEMENT_3D('',#4873,#3912,#3913);
#3509=AXIS2_PLACEMENT_3D('',#4877,#3915,#3916);
#3510=AXIS2_PLACEMENT_3D('',#4879,#3918,#3919);
#3511=AXIS2_PLACEMENT_3D('',#4881,#3920,#3921);
#3512=AXIS2_PLACEMENT_3D('',#4884,#3923,#3924);
#3513=AXIS2_PLACEMENT_3D('',#4886,#3925,#3926);
#3514=AXIS2_PLACEMENT_3D('',#4887,#3927,#3928);
#3515=AXIS2_PLACEMENT_3D('',#4888,#3929,#3930);
#3516=AXIS2_PLACEMENT_3D('',#4890,#3932,#3933);
#3517=AXIS2_PLACEMENT_3D('',#4892,#3935,#3936);
#3518=AXIS2_PLACEMENT_3D('',#4894,#3938,#3939);
#3519=AXIS2_PLACEMENT_3D('',#4895,#3940,#3941);
#3520=AXIS2_PLACEMENT_3D('',#4896,#3942,#3943);
#3521=AXIS2_PLACEMENT_3D('',#4898,#3944,#3945);
#3522=AXIS2_PLACEMENT_3D('',#4901,#3947,#3948);
#3523=AXIS2_PLACEMENT_3D('',#4902,#3949,#3950);
#3524=AXIS2_PLACEMENT_3D('',#4905,#3952,#3953);
#3525=AXIS2_PLACEMENT_3D('',#4906,#3954,#3955);
#3526=AXIS2_PLACEMENT_3D('',#4908,#3956,#3957);
#3527=AXIS2_PLACEMENT_3D('',#4909,#3958,#3959);
#3528=AXIS2_PLACEMENT_3D('',#4912,#3961,#3962);
#3529=AXIS2_PLACEMENT_3D('',#4913,#3963,#3964);
#3530=AXIS2_PLACEMENT_3D('',#4914,#3965,#3966);
#3531=AXIS2_PLACEMENT_3D('',#4915,#3967,#3968);
#3532=AXIS2_PLACEMENT_3D('',#4917,#3969,#3970);
#3533=AXIS2_PLACEMENT_3D('',#4919,#3971,#3972);
#3534=AXIS2_PLACEMENT_3D('',#4920,#3973,#3974);
#3535=AXIS2_PLACEMENT_3D('',#4923,#3976,#3977);
#3536=AXIS2_PLACEMENT_3D('',#4924,#3978,#3979);
#3537=AXIS2_PLACEMENT_3D('',#4925,#3980,#3981);
#3538=AXIS2_PLACEMENT_3D('',#4927,#3982,#3983);
#3539=AXIS2_PLACEMENT_3D('',#4928,#3984,#3985);
#3540=AXIS2_PLACEMENT_3D('',#4930,#3986,#3987);
#3541=AXIS2_PLACEMENT_3D('',#4932,#3989,#3990);
#3542=AXIS2_PLACEMENT_3D('',#4934,#3991,#3992);
#3543=AXIS2_PLACEMENT_3D('',#4936,#3994,#3995);
#3544=AXIS2_PLACEMENT_3D('',#4938,#3996,#3997);
#3545=AXIS2_PLACEMENT_3D('',#4940,#3999,#4000);
#3546=AXIS2_PLACEMENT_3D('',#4942,#4001,#4002);
#3547=AXIS2_PLACEMENT_3D('',#4943,#4003,#4004);
#3548=AXIS2_PLACEMENT_3D('',#4945,#4005,#4006);
#3549=AXIS2_PLACEMENT_3D('',#4947,#4008,#4009);
#3550=AXIS2_PLACEMENT_3D('',#4949,#4011,#4012);
#3551=AXIS2_PLACEMENT_3D('',#4958,#4017,#4018);
#3552=AXIS2_PLACEMENT_3D('',#4964,#4022,#4023);
#3553=AXIS2_PLACEMENT_3D('',#4970,#4027,#4028);
#3554=AXIS2_PLACEMENT_3D('',#4976,#4032,#4033);
#3555=AXIS2_PLACEMENT_3D('',#4982,#4037,#4038);
#3556=AXIS2_PLACEMENT_3D('',#4985,#4041,#4042);
#3557=AXIS2_PLACEMENT_3D('',#4986,#4043,#4044);
#3558=AXIS2_PLACEMENT_3D('',#4987,#4045,#4046);
#3559=AXIS2_PLACEMENT_3D('',#4988,#4047,#4048);
#3560=AXIS2_PLACEMENT_3D('',#4997,#4053,#4054);
#3561=AXIS2_PLACEMENT_3D('',#5003,#4058,#4059);
#3562=AXIS2_PLACEMENT_3D('',#5009,#4063,#4064);
#3563=AXIS2_PLACEMENT_3D('',#5015,#4068,#4069);
#3564=AXIS2_PLACEMENT_3D('',#5021,#4073,#4074);
#3565=AXIS2_PLACEMENT_3D('',#5027,#4078,#4079);
#3566=AXIS2_PLACEMENT_3D('',#5033,#4083,#4084);
#3567=AXIS2_PLACEMENT_3D('',#5039,#4088,#4089);
#3568=AXIS2_PLACEMENT_3D('',#5045,#4093,#4094);
#3569=AXIS2_PLACEMENT_3D('',#5054,#4099,#4100);
#3570=AXIS2_PLACEMENT_3D('',#5060,#4104,#4105);
#3571=AXIS2_PLACEMENT_3D('',#5066,#4109,#4110);
#3572=AXIS2_PLACEMENT_3D('',#5072,#4114,#4115);
#3573=AXIS2_PLACEMENT_3D('',#5078,#4119,#4120);
#3574=AXIS2_PLACEMENT_3D('',#5084,#4124,#4125);
#3575=AXIS2_PLACEMENT_3D('',#5090,#4129,#4130);
#3576=AXIS2_PLACEMENT_3D('',#5096,#4134,#4135);
#3577=AXIS2_PLACEMENT_3D('',#5102,#4139,#4140);
#3578=AXIS2_PLACEMENT_3D('',#5111,#4145,#4146);
#3579=AXIS2_PLACEMENT_3D('',#5117,#4150,#4151);
#3580=AXIS2_PLACEMENT_3D('',#5123,#4155,#4156);
#3581=AXIS2_PLACEMENT_3D('',#5129,#4160,#4161);
#3582=AXIS2_PLACEMENT_3D('',#5135,#4165,#4166);
#3583=AXIS2_PLACEMENT_3D('',#5141,#4170,#4171);
#3584=AXIS2_PLACEMENT_3D('',#5147,#4175,#4176);
#3585=AXIS2_PLACEMENT_3D('',#5153,#4180,#4181);
#3586=AXIS2_PLACEMENT_3D('',#5159,#4185,#4186);
#3587=AXIS2_PLACEMENT_3D('',#5168,#4191,#4192);
#3588=AXIS2_PLACEMENT_3D('',#5174,#4196,#4197);
#3589=AXIS2_PLACEMENT_3D('',#5180,#4201,#4202);
#3590=AXIS2_PLACEMENT_3D('',#5186,#4206,#4207);
#3591=AXIS2_PLACEMENT_3D('',#5192,#4211,#4212);
#3592=AXIS2_PLACEMENT_3D('',#5198,#4216,#4217);
#3593=AXIS2_PLACEMENT_3D('',#5204,#4221,#4222);
#3594=AXIS2_PLACEMENT_3D('',#5210,#4226,#4227);
#3595=AXIS2_PLACEMENT_3D('',#5216,#4231,#4232);
#3596=AXIS2_PLACEMENT_3D('',#5218,#4233,#4234);
#3597=AXIS2_PLACEMENT_3D('',#5221,#4236,#4237);
#3598=AXIS2_PLACEMENT_3D('',#5222,#4238,#4239);
#3599=AXIS2_PLACEMENT_3D('',#5228,#4243,#4244);
#3600=AXIS2_PLACEMENT_3D('',#5234,#4248,#4249);
#3601=AXIS2_PLACEMENT_3D('',#5237,#4252,#4253);
#3602=AXIS2_PLACEMENT_3D('',#5243,#4257,#4258);
#3603=AXIS2_PLACEMENT_3D('',#5246,#4261,#4262);
#3604=AXIS2_PLACEMENT_3D('',#5252,#4266,#4267);
#3605=AXIS2_PLACEMENT_3D('',#5255,#4270,#4271);
#3606=AXIS2_PLACEMENT_3D('',#5258,#4274,#4275);
#3607=AXIS2_PLACEMENT_3D('',#5259,#4276,#4277);
#3608=AXIS2_PLACEMENT_3D('',#5260,#4278,#4279);
#3609=AXIS2_PLACEMENT_3D('',#5261,#4280,#4281);
#3610=AXIS2_PLACEMENT_3D('',#5263,#4282,#4283);
#3611=AXIS2_PLACEMENT_3D('',#5266,#4285,#4286);
#3612=AXIS2_PLACEMENT_3D('',#5267,#4287,#4288);
#3613=AXIS2_PLACEMENT_3D('',#5269,#4289,#4290);
#3614=AXIS2_PLACEMENT_3D('',#5271,#4292,#4293);
#3615=AXIS2_PLACEMENT_3D('',#5272,#4294,#4295);
#3616=AXIS2_PLACEMENT_3D('',#5274,#4296,#4297);
#3617=AXIS2_PLACEMENT_3D('',#5300,#4299,#4300);
#3618=AXIS2_PLACEMENT_3D('',#5306,#4304,#4305);
#3619=AXIS2_PLACEMENT_3D('',#5310,#4308,#4309);
#3620=AXIS2_PLACEMENT_3D('',#5314,#4312,#4313);
#3621=AXIS2_PLACEMENT_3D('',#5318,#4316,#4317);
#3622=AXIS2_PLACEMENT_3D('',#5322,#4320,#4321);
#3623=AXIS2_PLACEMENT_3D('',#5324,#4323,#4324);
#3624=AXIS2_PLACEMENT_3D('',#5325,#4325,#4326);
#3625=AXIS2_PLACEMENT_3D('',#5326,#4327,#4328);
#3626=AXIS2_PLACEMENT_3D('',#5327,#4329,#4330);
#3627=AXIS2_PLACEMENT_3D('',#5328,#4331,#4332);
#3628=AXIS2_PLACEMENT_3D('',#5330,#4333,#4334);
#3629=AXIS2_PLACEMENT_3D('',#5333,#4336,#4337);
#3630=AXIS2_PLACEMENT_3D('',#5334,#4338,#4339);
#3631=AXIS2_PLACEMENT_3D('',#5336,#4340,#4341);
#3632=AXIS2_PLACEMENT_3D('',#5339,#4343,#4344);
#3633=AXIS2_PLACEMENT_3D('',#5340,#4345,#4346);
#3634=AXIS2_PLACEMENT_3D('',#5343,#4347,#4348);
#3635=AXIS2_PLACEMENT_3D('',#5345,#4349,#4350);
#3636=AXIS2_PLACEMENT_3D('',#5352,#4354,#4355);
#3637=AXIS2_PLACEMENT_3D('',#5353,#4356,#4357);
#3638=AXIS2_PLACEMENT_3D('',#5359,#4361,#4362);
#3639=AXIS2_PLACEMENT_3D('',#5363,#4365,#4366);
#3640=AXIS2_PLACEMENT_3D('',#5367,#4369,#4370);
#3641=AXIS2_PLACEMENT_3D('',#5368,#4371,#4372);
#3642=AXIS2_PLACEMENT_3D('',#5369,#4373,#4374);
#3643=AXIS2_PLACEMENT_3D('',#5372,#4376,#4377);
#3644=AXIS2_PLACEMENT_3D('',#5373,#4378,#4379);
#3645=AXIS2_PLACEMENT_3D('',#5376,#4381,#4382);
#3646=AXIS2_PLACEMENT_3D('',#5377,#4383,#4384);
#3647=AXIS2_PLACEMENT_3D('',#5378,#4385,#4386);
#3648=AXIS2_PLACEMENT_3D('',#5379,#4387,#4388);
#3649=AXIS2_PLACEMENT_3D('',#5381,#4389,#4390);
#3650=AXIS2_PLACEMENT_3D('',#5384,#4392,#4393);
#3651=AXIS2_PLACEMENT_3D('',#5385,#4394,#4395);
#3652=AXIS2_PLACEMENT_3D('',#5387,#4396,#4397);
#3653=AXIS2_PLACEMENT_3D('',#5388,#4398,#4399);
#3654=AXIS2_PLACEMENT_3D('',#5390,#4400,#4401);
#3655=AXIS2_PLACEMENT_3D('',#5393,#4403,#4404);
#3656=AXIS2_PLACEMENT_3D('',#5394,#4405,#4406);
#3657=AXIS2_PLACEMENT_3D('',#5396,#4407,#4408);
#3658=AXIS2_PLACEMENT_3D('',#5397,#4409,#4410);
#3659=AXIS2_PLACEMENT_3D('',#5399,#4411,#4412);
#3660=AXIS2_PLACEMENT_3D('',#5401,#4414,#4415);
#3661=AXIS2_PLACEMENT_3D('',#5403,#4416,#4417);
#3662=AXIS2_PLACEMENT_3D('',#5405,#4419,#4420);
#3663=AXIS2_PLACEMENT_3D('',#5414,#4425,#4426);
#3664=AXIS2_PLACEMENT_3D('',#5420,#4430,#4431);
#3665=AXIS2_PLACEMENT_3D('',#5426,#4435,#4436);
#3666=AXIS2_PLACEMENT_3D('',#5429,#4439,#4440);
#3667=AXIS2_PLACEMENT_3D('',#5430,#4441,#4442);
#3668=AXIS2_PLACEMENT_3D('',#5431,#4443,#4444);
#3669=AXIS2_PLACEMENT_3D('',#5432,#4445,#4446);
#3670=AXIS2_PLACEMENT_3D('',#5434,#4447,#4448);
#3671=AXIS2_PLACEMENT_3D('',#5435,#4449,#4450);
#3672=AXIS2_PLACEMENT_3D('',#5437,#4451,#4452);
#3673=AXIS2_PLACEMENT_3D('',#5439,#4454,#4455);
#3674=AXIS2_PLACEMENT_3D('',#5441,#4456,#4457);
#3675=AXIS2_PLACEMENT_3D('',#5443,#4459,#4460);
#3676=AXIS2_PLACEMENT_3D('',#5445,#4461,#4462);
#3677=AXIS2_PLACEMENT_3D('',#5447,#4464,#4465);
#3678=AXIS2_PLACEMENT_3D('',#5449,#4466,#4467);
#3679=AXIS2_PLACEMENT_3D('',#5450,#4468,#4469);
#3680=AXIS2_PLACEMENT_3D('',#5452,#4470,#4471);
#3681=AXIS2_PLACEMENT_3D('',#5454,#4473,#4474);
#3682=AXIS2_PLACEMENT_3D('',#5456,#4475,#4476);
#3683=AXIS2_PLACEMENT_3D('',#5458,#4478,#4479);
#3684=AXIS2_PLACEMENT_3D('',#5460,#4480,#4481);
#3685=AXIS2_PLACEMENT_3D('',#5462,#4483,#4484);
#3686=AXIS2_PLACEMENT_3D('',#5463,#4485,#4486);
#3687=AXIS2_PLACEMENT_3D('',#5472,#4491,#4492);
#3688=AXIS2_PLACEMENT_3D('',#5478,#4496,#4497);
#3689=AXIS2_PLACEMENT_3D('',#5484,#4501,#4502);
#3690=AXIS2_PLACEMENT_3D('',#5490,#4506,#4507);
#3691=AXIS2_PLACEMENT_3D('',#5496,#4511,#4512);
#3692=AXIS2_PLACEMENT_3D('',#5499,#4515,#4516);
#3693=AXIS2_PLACEMENT_3D('',#5500,#4517,#4518);
#3694=AXIS2_PLACEMENT_3D('',#5501,#4519,#4520);
#3695=AXIS2_PLACEMENT_3D('',#5502,#4521,#4522);
#3696=AXIS2_PLACEMENT_3D('',#5504,#4523,#4524);
#3697=AXIS2_PLACEMENT_3D('',#5507,#4526,#4527);
#3698=AXIS2_PLACEMENT_3D('',#5508,#4528,#4529);
#3699=AXIS2_PLACEMENT_3D('',#5510,#4530,#4531);
#3700=AXIS2_PLACEMENT_3D('',#5513,#4533,#4534);
#3701=AXIS2_PLACEMENT_3D('',#5514,#4535,#4536);
#3702=AXIS2_PLACEMENT_3D('',#5515,#4537,#4538);
#3703=AXIS2_PLACEMENT_3D('',#5516,#4539,#4540);
#3704=AXIS2_PLACEMENT_3D('',#5517,#4541,#4542);
#3705=AXIS2_PLACEMENT_3D('',#5518,#4543,#4544);
#3706=AXIS2_PLACEMENT_3D('',#5519,#4545,#4546);
#3707=AXIS2_PLACEMENT_3D('',#5520,#4547,#4548);
#3708=AXIS2_PLACEMENT_3D('',#5521,#4549,#4550);
#3709=AXIS2_PLACEMENT_3D('',#5522,#4551,#4552);
#3710=AXIS2_PLACEMENT_3D('',#5523,#4553,#4554);
#3711=AXIS2_PLACEMENT_3D('',#5524,#4555,#4556);
#3712=AXIS2_PLACEMENT_3D('',#5525,#4557,#4558);
#3713=AXIS2_PLACEMENT_3D('',#5526,#4559,#4560);
#3714=AXIS2_PLACEMENT_3D('',#5527,#4561,#4562);
#3715=AXIS2_PLACEMENT_3D('',#5539,#4564,#4565);
#3716=AXIS2_PLACEMENT_3D('',#5555,#4566,#4567);
#3717=AXIS2_PLACEMENT_3D('',#5557,#4568,#4569);
#3718=AXIS2_PLACEMENT_3D('',#5583,#4571,#4572);
#3719=AXIS2_PLACEMENT_3D('',#5586,#4575,#4576);
#3720=AXIS2_PLACEMENT_3D('',#5588,#4578,#4579);
#3721=AXIS2_PLACEMENT_3D('',#5590,#4581,#4582);
#3722=AXIS2_PLACEMENT_3D('',#5592,#4583,#4584);
#3723=AXIS2_PLACEMENT_3D('',#5595,#4586,#4587);
#3724=AXIS2_PLACEMENT_3D('',#5596,#4588,#4589);
#3725=AXIS2_PLACEMENT_3D('',#5598,#4591,#4592);
#3726=AXIS2_PLACEMENT_3D('',#5600,#4594,#4595);
#3727=AXIS2_PLACEMENT_3D('',#5601,#4596,#4597);
#3728=AXIS2_PLACEMENT_3D('',#5602,#4598,#4599);
#3729=AXIS2_PLACEMENT_3D('',#5603,#4600,#4601);
#3730=AXIS2_PLACEMENT_3D('',#5604,#4602,#4603);
#3731=AXIS2_PLACEMENT_3D('',#5609,#4605,#4606);
#3732=AXIS2_PLACEMENT_3D('',#5612,#4608,#4609);
#3733=AXIS2_PLACEMENT_3D('',#5613,#4610,#4611);
#3734=AXIS2_PLACEMENT_3D('',#5618,#4613,#4614);
#3735=AXIS2_PLACEMENT_3D('',#5621,#4616,#4617);
#3736=AXIS2_PLACEMENT_3D('',#5622,#4618,#4619);
#3737=AXIS2_PLACEMENT_3D('',#5627,#4621,#4622);
#3738=AXIS2_PLACEMENT_3D('',#5630,#4624,#4625);
#3739=AXIS2_PLACEMENT_3D('',#5631,#4626,#4627);
#3740=AXIS2_PLACEMENT_3D('',#5636,#4629,#4630);
#3741=AXIS2_PLACEMENT_3D('',#5639,#4632,#4633);
#3742=AXIS2_PLACEMENT_3D('',#5640,#4634,#4635);
#3743=AXIS2_PLACEMENT_3D('',#5645,#4637,#4638);
#3744=AXIS2_PLACEMENT_3D('',#5648,#4640,#4641);
#3745=AXIS2_PLACEMENT_3D('',#5649,#4642,#4643);
#3746=AXIS2_PLACEMENT_3D('',#5654,#4645,#4646);
#3747=AXIS2_PLACEMENT_3D('',#5657,#4648,#4649);
#3748=AXIS2_PLACEMENT_3D('',#5658,#4650,#4651);
#3749=AXIS2_PLACEMENT_3D('',#5659,#4652,#4653);
#3750=AXIS2_PLACEMENT_3D('',#5660,#4654,#4655);
#3751=AXIS2_PLACEMENT_3D('',#5661,#4656,#4657);
#3752=AXIS2_PLACEMENT_3D('',#5662,#4658,#4659);
#3753=AXIS2_PLACEMENT_3D('',#5663,#4660,#4661);
#3754=AXIS2_PLACEMENT_3D('',#5664,#4662,#4663);
#3755=AXIS2_PLACEMENT_3D('',#5666,#4664,#4665);
#3756=AXIS2_PLACEMENT_3D('',#5667,#4666,#4667);
#3757=AXIS2_PLACEMENT_3D('',#5668,#4668,#4669);
#3758=AXIS2_PLACEMENT_3D('',#5669,#4670,#4671);
#3759=AXIS2_PLACEMENT_3D('',#5670,#4672,#4673);
#3760=AXIS2_PLACEMENT_3D('',#5671,#4674,#4675);
#3761=AXIS2_PLACEMENT_3D('',#5672,#4676,#4677);
#3762=AXIS2_PLACEMENT_3D('',#5673,#4678,#4679);
#3763=AXIS2_PLACEMENT_3D('',#5674,#4680,#4681);
#3764=AXIS2_PLACEMENT_3D('',#5675,#4682,#4683);
#3765=AXIS2_PLACEMENT_3D('',#5676,#4684,#4685);
#3766=AXIS2_PLACEMENT_3D('',#5677,#4686,#4687);
#3767=AXIS2_PLACEMENT_3D('',#5678,#4688,#4689);
#3768=AXIS2_PLACEMENT_3D('',#5679,#4690,#4691);
#3769=AXIS2_PLACEMENT_3D('',#5688,#4696,#4697);
#3770=AXIS2_PLACEMENT_3D('',#5694,#4701,#4702);
#3771=AXIS2_PLACEMENT_3D('',#5700,#4706,#4707);
#3772=AXIS2_PLACEMENT_3D('',#5706,#4711,#4712);
#3773=AXIS2_PLACEMENT_3D('',#5712,#4716,#4717);
#3774=AXIS2_PLACEMENT_3D('',#5715,#4720,#4721);
#3775=AXIS2_PLACEMENT_3D('',#5717,#4722,#4723);
#3776=AXIS2_PLACEMENT_3D('',#5718,#4724,#4725);
#3777=AXIS2_PLACEMENT_3D('',#5720,#4727,#4728);
#3778=AXIS2_PLACEMENT_3D('',#5721,#4729,#4730);
#3779=AXIS2_PLACEMENT_3D('',#5722,#4731,#4732);
#3780=AXIS2_PLACEMENT_3D('',#5723,#4733,#4734);
#3781=AXIS2_PLACEMENT_3D('',#5724,#4735,#4736);
#3782=AXIS2_PLACEMENT_3D('',#5725,#4737,#4738);
#3783=AXIS2_PLACEMENT_3D('',#5726,#4739,#4740);
#3784=AXIS2_PLACEMENT_3D('',#5727,#4741,#4742);
#3785=AXIS2_PLACEMENT_3D('',#5728,#4743,#4744);
#3786=AXIS2_PLACEMENT_3D('',#5729,#4745,#4746);
#3787=DIRECTION('axis',(0.,0.,1.));
#3788=DIRECTION('refdir',(1.,0.,0.));
#3789=DIRECTION('axis',(0.,0.,1.));
#3790=DIRECTION('refdir',(1.,0.,0.));
#3791=DIRECTION('axis',(0.,0.,1.));
#3792=DIRECTION('refdir',(1.,0.,0.));
#3793=DIRECTION('center_axis',(0.,0.,1.));
#3794=DIRECTION('ref_axis',(1.,0.,0.));
#3795=DIRECTION('center_axis',(0.,0.,1.));
#3796=DIRECTION('ref_axis',(1.,0.,0.));
#3797=DIRECTION('',(0.,0.,-1.));
#3798=DIRECTION('center_axis',(0.,0.,1.));
#3799=DIRECTION('ref_axis',(1.,0.,0.));
#3800=DIRECTION('center_axis',(0.,0.,1.));
#3801=DIRECTION('ref_axis',(1.,0.,0.));
#3802=DIRECTION('center_axis',(0.,0.,-1.));
#3803=DIRECTION('ref_axis',(1.,0.,0.));
#3804=DIRECTION('center_axis',(0.,0.,1.));
#3805=DIRECTION('ref_axis',(1.,0.,0.));
#3806=DIRECTION('center_axis',(0.,0.,1.));
#3807=DIRECTION('ref_axis',(1.,0.,0.));
#3808=DIRECTION('',(0.,0.,-1.));
#3809=DIRECTION('center_axis',(0.,0.,1.));
#3810=DIRECTION('ref_axis',(1.,0.,0.));
#3811=DIRECTION('center_axis',(0.,0.,1.));
#3812=DIRECTION('ref_axis',(1.,0.,0.));
#3813=DIRECTION('center_axis',(0.,0.,-1.));
#3814=DIRECTION('ref_axis',(1.,0.,0.));
#3815=DIRECTION('center_axis',(0.,0.,1.));
#3816=DIRECTION('ref_axis',(1.,0.,0.));
#3817=DIRECTION('',(0.,0.,1.));
#3818=DIRECTION('center_axis',(0.,0.,-1.));
#3819=DIRECTION('ref_axis',(1.,0.,0.));
#3820=DIRECTION('center_axis',(0.,0.,1.));
#3821=DIRECTION('ref_axis',(1.,0.,0.));
#3822=DIRECTION('',(0.,0.,1.));
#3823=DIRECTION('center_axis',(0.,0.,-1.));
#3824=DIRECTION('ref_axis',(1.,0.,0.));
#3825=DIRECTION('center_axis',(0.,0.,1.));
#3826=DIRECTION('ref_axis',(1.,0.,0.));
#3827=DIRECTION('center_axis',(0.,0.,1.));
#3828=DIRECTION('ref_axis',(1.,0.,0.));
#3829=DIRECTION('',(0.,0.,1.));
#3830=DIRECTION('center_axis',(0.,0.,-1.));
#3831=DIRECTION('ref_axis',(1.,0.,0.));
#3832=DIRECTION('center_axis',(0.,0.,1.));
#3833=DIRECTION('ref_axis',(1.,0.,0.));
#3834=DIRECTION('center_axis',(0.,0.,1.));
#3835=DIRECTION('ref_axis',(1.,0.,0.));
#3836=DIRECTION('',(0.,0.,-1.));
#3837=DIRECTION('center_axis',(0.,0.,-1.));
#3838=DIRECTION('ref_axis',(1.,0.,0.));
#3839=DIRECTION('center_axis',(0.,0.,1.));
#3840=DIRECTION('ref_axis',(1.,0.,0.));
#3841=DIRECTION('center_axis',(0.,1.,0.));
#3842=DIRECTION('ref_axis',(-1.,0.,0.));
#3843=DIRECTION('',(-1.,0.,0.));
#3844=DIRECTION('',(0.,0.,1.));
#3845=DIRECTION('',(-1.,0.,0.));
#3846=DIRECTION('',(0.,0.,1.));
#3847=DIRECTION('center_axis',(1.,0.,0.));
#3848=DIRECTION('ref_axis',(0.,1.,0.));
#3849=DIRECTION('',(0.,1.,0.));
#3850=DIRECTION('',(0.,1.,0.));
#3851=DIRECTION('',(0.,0.,1.));
#3852=DIRECTION('center_axis',(0.,-1.,0.));
#3853=DIRECTION('ref_axis',(1.,0.,0.));
#3854=DIRECTION('',(1.,0.,0.));
#3855=DIRECTION('',(1.,0.,0.));
#3856=DIRECTION('',(0.,0.,1.));
#3857=DIRECTION('center_axis',(-1.,0.,0.));
#3858=DIRECTION('ref_axis',(0.,-1.,0.));
#3859=DIRECTION('',(0.,-1.,0.));
#3860=DIRECTION('',(0.,-1.,0.));
#3861=DIRECTION('center_axis',(0.,0.,1.));
#3862=DIRECTION('ref_axis',(1.,0.,0.));
#3863=DIRECTION('center_axis',(0.,0.,1.));
#3864=DIRECTION('ref_axis',(1.,0.,0.));
#3865=DIRECTION('axis',(0.,0.,1.));
#3866=DIRECTION('refdir',(1.,0.,0.));
#3867=DIRECTION('center_axis',(0.,0.,1.));
#3868=DIRECTION('ref_axis',(1.,0.,0.));
#3869=DIRECTION('',(1.,0.,0.));
#3870=DIRECTION('',(0.,-1.,0.));
#3871=DIRECTION('',(-1.,0.,0.));
#3872=DIRECTION('',(0.,1.,0.));
#3873=DIRECTION('center_axis',(0.,1.,0.));
#3874=DIRECTION('ref_axis',(-1.,0.,0.));
#3875=DIRECTION('',(0.,0.,1.));
#3876=DIRECTION('',(-1.,0.,0.));
#3877=DIRECTION('',(0.,0.,1.));
#3878=DIRECTION('center_axis',(0.,0.,1.));
#3879=DIRECTION('ref_axis',(1.,0.,0.));
#3880=DIRECTION('',(0.,-1.,0.));
#3881=DIRECTION('',(1.,0.,0.));
#3882=DIRECTION('',(0.,1.,0.));
#3883=DIRECTION('center_axis',(0.,0.,-1.));
#3884=DIRECTION('ref_axis',(1.,0.,0.));
#3885=DIRECTION('center_axis',(-1.,0.,0.));
#3886=DIRECTION('ref_axis',(0.,-1.,0.));
#3887=DIRECTION('',(0.,0.,1.));
#3888=DIRECTION('',(0.,0.707106781186548,0.707106781186548));
#3889=DIRECTION('',(0.,-1.,0.));
#3890=DIRECTION('',(0.,0.707106781186548,-0.707106781186548));
#3891=DIRECTION('',(0.,0.,1.));
#3892=DIRECTION('',(0.,-1.,0.));
#3893=DIRECTION('',(0.,0.,1.));
#3894=DIRECTION('center_axis',(0.,-1.,0.));
#3895=DIRECTION('ref_axis',(1.,0.,0.));
#3896=DIRECTION('',(1.,0.,0.));
#3897=DIRECTION('',(0.,0.,1.));
#3898=DIRECTION('center_axis',(0.,0.,1.));
#3899=DIRECTION('ref_axis',(1.,0.,0.));
#3900=DIRECTION('',(-1.,0.,0.));
#3901=DIRECTION('',(0.,1.,0.));
#3902=DIRECTION('center_axis',(1.,0.,0.));
#3903=DIRECTION('ref_axis',(0.,1.,0.));
#3904=DIRECTION('',(0.,0.,1.));
#3905=DIRECTION('',(0.,-0.707106781186548,0.707106781186548));
#3906=DIRECTION('',(0.,1.,0.));
#3907=DIRECTION('',(0.,-0.707106781186548,-0.707106781186548));
#3908=DIRECTION('',(0.,0.,1.));
#3909=DIRECTION('center_axis',(0.,-1.,0.));
#3910=DIRECTION('ref_axis',(1.,0.,0.));
#3911=DIRECTION('',(-1.,0.,0.));
#3912=DIRECTION('center_axis',(0.,-0.707106781186548,-0.707106781186548));
#3913=DIRECTION('ref_axis',(-1.,0.,0.));
#3914=DIRECTION('',(1.,0.,0.));
#3915=DIRECTION('center_axis',(0.,0.707106781186548,0.707106781186548));
#3916=DIRECTION('ref_axis',(0.,0.707106781186547,-0.707106781186547));
#3917=DIRECTION('',(1.,0.,0.));
#3918=DIRECTION('center_axis',(0.,0.,1.));
#3919=DIRECTION('ref_axis',(1.,0.,0.));
#3920=DIRECTION('center_axis',(0.,0.,-1.));
#3921=DIRECTION('ref_axis',(1.,0.,0.));
#3922=DIRECTION('',(0.,0.,1.));
#3923=DIRECTION('center_axis',(0.,0.,-1.));
#3924=DIRECTION('ref_axis',(1.,0.,0.));
#3925=DIRECTION('center_axis',(0.,-0.707106781186548,0.707106781186548));
#3926=DIRECTION('ref_axis',(0.,0.707106781186547,0.707106781186547));
#3927=DIRECTION('center_axis',(0.,0.,-1.));
#3928=DIRECTION('ref_axis',(1.,0.,0.));
#3929=DIRECTION('center_axis',(0.,0.,1.));
#3930=DIRECTION('ref_axis',(1.,0.,0.));
#3931=DIRECTION('',(-1.,0.,0.));
#3932=DIRECTION('center_axis',(0.,0.,1.));
#3933=DIRECTION('ref_axis',(1.,0.,0.));
#3934=DIRECTION('',(-1.,0.,0.));
#3935=DIRECTION('center_axis',(0.,0.707106781186548,-0.707106781186548));
#3936=DIRECTION('ref_axis',(-1.,0.,0.));
#3937=DIRECTION('',(1.,0.,0.));
#3938=DIRECTION('center_axis',(0.,1.,0.));
#3939=DIRECTION('ref_axis',(-1.,0.,0.));
#3940=DIRECTION('axis',(0.,0.,1.));
#3941=DIRECTION('refdir',(1.,0.,0.));
#3942=DIRECTION('center_axis',(0.,1.,0.));
#3943=DIRECTION('ref_axis',(1.,0.,0.));
#3944=DIRECTION('center_axis',(0.,1.,0.));
#3945=DIRECTION('ref_axis',(1.,0.,0.));
#3946=DIRECTION('',(0.707106781186548,-0.707106781186547,-8.65956056235494E-17));
#3947=DIRECTION('center_axis',(0.,-1.,0.));
#3948=DIRECTION('ref_axis',(1.,0.,0.));
#3949=DIRECTION('center_axis',(0.,1.,0.));
#3950=DIRECTION('ref_axis',(1.,0.,0.));
#3951=DIRECTION('',(0.,-1.,0.));
#3952=DIRECTION('center_axis',(0.,-1.,0.));
#3953=DIRECTION('ref_axis',(1.,0.,0.));
#3954=DIRECTION('center_axis',(0.,1.,0.));
#3955=DIRECTION('ref_axis',(1.,0.,0.));
#3956=DIRECTION('center_axis',(0.,1.,0.));
#3957=DIRECTION('ref_axis',(1.,0.,0.));
#3958=DIRECTION('center_axis',(0.,1.,0.));
#3959=DIRECTION('ref_axis',(1.,0.,0.));
#3960=DIRECTION('',(0.,-1.,0.));
#3961=DIRECTION('center_axis',(0.,1.,0.));
#3962=DIRECTION('ref_axis',(1.,0.,0.));
#3963=DIRECTION('center_axis',(0.,1.,0.));
#3964=DIRECTION('ref_axis',(1.,0.,0.));
#3965=DIRECTION('axis',(0.,0.,1.));
#3966=DIRECTION('refdir',(1.,0.,0.));
#3967=DIRECTION('center_axis',(0.,1.,0.));
#3968=DIRECTION('ref_axis',(1.,0.,0.));
#3969=DIRECTION('center_axis',(0.,1.,0.));
#3970=DIRECTION('ref_axis',(1.,0.,0.));
#3971=DIRECTION('center_axis',(0.,1.,0.));
#3972=DIRECTION('ref_axis',(1.,0.,0.));
#3973=DIRECTION('center_axis',(0.,1.,0.));
#3974=DIRECTION('ref_axis',(1.,0.,0.));
#3975=DIRECTION('',(0.,-1.,0.));
#3976=DIRECTION('center_axis',(0.,1.,0.));
#3977=DIRECTION('ref_axis',(1.,0.,0.));
#3978=DIRECTION('center_axis',(0.,1.,0.));
#3979=DIRECTION('ref_axis',(1.,0.,0.));
#3980=DIRECTION('center_axis',(0.,1.,0.));
#3981=DIRECTION('ref_axis',(0.,0.,1.));
#3982=DIRECTION('center_axis',(0.,-1.,0.));
#3983=DIRECTION('ref_axis',(1.,0.,0.));
#3984=DIRECTION('center_axis',(0.,-1.,0.));
#3985=DIRECTION('ref_axis',(1.,0.,0.));
#3986=DIRECTION('center_axis',(0.,-1.,0.));
#3987=DIRECTION('ref_axis',(1.,0.,0.));
#3988=DIRECTION('',(0.707106781186548,0.707106781186547,8.65956056235493E-17));
#3989=DIRECTION('center_axis',(0.,-1.,0.));
#3990=DIRECTION('ref_axis',(1.,0.,0.));
#3991=DIRECTION('center_axis',(0.,-1.,0.));
#3992=DIRECTION('ref_axis',(1.,0.,0.));
#3993=DIRECTION('',(0.,1.,0.));
#3994=DIRECTION('center_axis',(0.,1.,0.));
#3995=DIRECTION('ref_axis',(1.,0.,0.));
#3996=DIRECTION('center_axis',(0.,-1.,0.));
#3997=DIRECTION('ref_axis',(1.,0.,0.));
#3998=DIRECTION('',(-0.707106781186547,0.707106781186548,-8.65956056235493E-17));
#3999=DIRECTION('center_axis',(0.,-1.,0.));
#4000=DIRECTION('ref_axis',(0.,0.,-1.));
#4001=DIRECTION('center_axis',(0.,-1.,0.));
#4002=DIRECTION('ref_axis',(1.,0.,0.));
#4003=DIRECTION('center_axis',(0.,1.,0.));
#4004=DIRECTION('ref_axis',(1.,0.,0.));
#4005=DIRECTION('center_axis',(0.,1.,0.));
#4006=DIRECTION('ref_axis',(1.,0.,0.));
#4007=DIRECTION('',(-0.447213595499958,0.894427190999916,-5.47678698264203E-17));
#4008=DIRECTION('center_axis',(0.,-1.,0.));
#4009=DIRECTION('ref_axis',(1.,0.,0.));
#4010=DIRECTION('',(0.,1.,0.));
#4011=DIRECTION('center_axis',(0.866025403784439,0.,-0.5));
#4012=DIRECTION('ref_axis',(0.5,0.,0.866025403784439));
#4013=DIRECTION('',(-0.5,0.,-0.866025403784439));
#4014=DIRECTION('',(0.,-1.,0.));
#4015=DIRECTION('',(0.5,0.,0.866025403784439));
#4016=DIRECTION('',(0.,-1.,0.));
#4017=DIRECTION('center_axis',(1.20185167898973E-16,0.,-1.));
#4018=DIRECTION('ref_axis',(1.,0.,1.20185167898973E-16));
#4019=DIRECTION('',(-1.,0.,-1.20185167898973E-16));
#4020=DIRECTION('',(0.,-1.,0.));
#4021=DIRECTION('',(1.,0.,1.20185167898973E-16));
#4022=DIRECTION('center_axis',(-0.866025403784439,0.,-0.5));
#4023=DIRECTION('ref_axis',(0.5,0.,-0.866025403784439));
#4024=DIRECTION('',(-0.5,0.,0.866025403784439));
#4025=DIRECTION('',(0.,-1.,0.));
#4026=DIRECTION('',(0.5,0.,-0.866025403784439));
#4027=DIRECTION('center_axis',(-0.866025403784439,0.,0.5));
#4028=DIRECTION('ref_axis',(-0.5,0.,-0.866025403784439));
#4029=DIRECTION('',(0.5,0.,0.866025403784439));
#4030=DIRECTION('',(0.,-1.,0.));
#4031=DIRECTION('',(-0.5,0.,-0.866025403784439));
#4032=DIRECTION('center_axis',(-2.40370335797945E-16,0.,1.));
#4033=DIRECTION('ref_axis',(-1.,0.,-2.40370335797945E-16));
#4034=DIRECTION('',(1.,0.,2.40370335797945E-16));
#4035=DIRECTION('',(0.,-1.,0.));
#4036=DIRECTION('',(-1.,0.,-2.40370335797945E-16));
#4037=DIRECTION('center_axis',(0.866025403784439,0.,0.5));
#4038=DIRECTION('ref_axis',(-0.5,0.,0.866025403784439));
#4039=DIRECTION('',(0.5,0.,-0.866025403784439));
#4040=DIRECTION('',(-0.5,0.,0.866025403784439));
#4041=DIRECTION('center_axis',(0.,1.,0.));
#4042=DIRECTION('ref_axis',(1.,0.,0.));
#4043=DIRECTION('center_axis',(0.,-1.,0.));
#4044=DIRECTION('ref_axis',(0.,0.,-1.));
#4045=DIRECTION('axis',(0.,0.,1.));
#4046=DIRECTION('refdir',(1.,0.,0.));
#4047=DIRECTION('center_axis',(0.,0.,-1.));
#4048=DIRECTION('ref_axis',(0.,1.,0.));
#4049=DIRECTION('',(0.,1.,0.));
#4050=DIRECTION('',(1.,0.,0.));
#4051=DIRECTION('',(0.,-1.,0.));
#4052=DIRECTION('',(1.,0.,0.));
#4053=DIRECTION('center_axis',(0.,1.,-8.88178419700125E-16));
#4054=DIRECTION('ref_axis',(0.,8.88178419700125E-16,1.));
#4055=DIRECTION('',(0.,8.88178419700125E-16,1.));
#4056=DIRECTION('',(1.,0.,0.));
#4057=DIRECTION('',(0.,-8.88178419700125E-16,-1.));
#4058=DIRECTION('center_axis',(0.,-7.40148683083439E-16,-1.));
#4059=DIRECTION('ref_axis',(0.,1.,-7.40148683083439E-16));
#4060=DIRECTION('',(0.,1.,-7.40148683083439E-16));
#4061=DIRECTION('',(1.,0.,0.));
#4062=DIRECTION('',(0.,-1.,7.40148683083439E-16));
#4063=DIRECTION('center_axis',(0.,-0.707106781186547,-0.707106781186548));
#4064=DIRECTION('ref_axis',(0.,0.707106781186548,-0.707106781186547));
#4065=DIRECTION('',(0.,0.707106781186548,-0.707106781186547));
#4066=DIRECTION('',(1.,0.,0.));
#4067=DIRECTION('',(0.,-0.707106781186548,0.707106781186547));
#4068=DIRECTION('center_axis',(0.,-1.,2.77555756156289E-16));
#4069=DIRECTION('ref_axis',(0.,-2.77555756156289E-16,-1.));
#4070=DIRECTION('',(0.,-2.77555756156289E-16,-1.));
#4071=DIRECTION('',(1.,0.,0.));
#4072=DIRECTION('',(0.,2.77555756156289E-16,1.));
#4073=DIRECTION('center_axis',(0.,-0.707106781186547,0.707106781186548));
#4074=DIRECTION('ref_axis',(0.,-0.707106781186548,-0.707106781186547));
#4075=DIRECTION('',(0.,-0.707106781186548,-0.707106781186547));
#4076=DIRECTION('',(1.,0.,0.));
#4077=DIRECTION('',(0.,0.707106781186548,0.707106781186547));
#4078=DIRECTION('center_axis',(0.,7.40148683083438E-16,1.));
#4079=DIRECTION('ref_axis',(0.,-1.,7.40148683083438E-16));
#4080=DIRECTION('',(0.,-1.,7.40148683083438E-16));
#4081=DIRECTION('',(1.,0.,0.));
#4082=DIRECTION('',(0.,1.,-7.40148683083438E-16));
#4083=DIRECTION('center_axis',(0.,1.,-4.44089209850063E-16));
#4084=DIRECTION('ref_axis',(0.,4.44089209850063E-16,1.));
#4085=DIRECTION('',(0.,4.44089209850063E-16,1.));
#4086=DIRECTION('',(1.,0.,0.));
#4087=DIRECTION('',(0.,-4.44089209850063E-16,-1.));
#4088=DIRECTION('center_axis',(0.,2.41352831440251E-16,1.));
#4089=DIRECTION('ref_axis',(0.,-1.,2.41352831440251E-16));
#4090=DIRECTION('',(0.,-1.,2.41352831440251E-16));
#4091=DIRECTION('',(-1.,0.,0.));
#4092=DIRECTION('',(0.,1.,-2.41352831440251E-16));
#4093=DIRECTION('center_axis',(0.,-1.,2.41352831440251E-16));
#4094=DIRECTION('ref_axis',(0.,-2.41352831440251E-16,-1.));
#4095=DIRECTION('',(0.,-2.41352831440251E-16,-1.));
#4096=DIRECTION('',(1.,0.,0.));
#4097=DIRECTION('',(0.,2.41352831440251E-16,1.));
#4098=DIRECTION('',(1.,0.,0.));
#4099=DIRECTION('center_axis',(0.,0.,-1.));
#4100=DIRECTION('ref_axis',(0.,1.,0.));
#4101=DIRECTION('',(0.,1.,0.));
#4102=DIRECTION('',(1.,0.,0.));
#4103=DIRECTION('',(0.,-1.,0.));
#4104=DIRECTION('center_axis',(0.,-1.,0.));
#4105=DIRECTION('ref_axis',(0.,0.,-1.));
#4106=DIRECTION('',(0.,0.,-1.));
#4107=DIRECTION('',(1.,0.,0.));
#4108=DIRECTION('',(0.,0.,1.));
#4109=DIRECTION('center_axis',(0.,-0.707106781186547,0.707106781186548));
#4110=DIRECTION('ref_axis',(0.,-0.707106781186548,-0.707106781186547));
#4111=DIRECTION('',(0.,-0.707106781186548,-0.707106781186547));
#4112=DIRECTION('',(1.,0.,0.));
#4113=DIRECTION('',(0.,0.707106781186548,0.707106781186547));
#4114=DIRECTION('center_axis',(0.,0.,1.));
#4115=DIRECTION('ref_axis',(0.,-1.,0.));
#4116=DIRECTION('',(0.,-1.,0.));
#4117=DIRECTION('',(1.,0.,0.));
#4118=DIRECTION('',(0.,1.,0.));
#4119=DIRECTION('center_axis',(0.,0.707106781186548,0.707106781186547));
#4120=DIRECTION('ref_axis',(0.,-0.707106781186547,0.707106781186548));
#4121=DIRECTION('',(0.,-0.707106781186547,0.707106781186548));
#4122=DIRECTION('',(1.,0.,0.));
#4123=DIRECTION('',(0.,0.707106781186547,-0.707106781186548));
#4124=DIRECTION('center_axis',(0.,1.,0.));
#4125=DIRECTION('ref_axis',(0.,0.,1.));
#4126=DIRECTION('',(0.,0.,1.));
#4127=DIRECTION('',(1.,0.,0.));
#4128=DIRECTION('',(0.,0.,-1.));
#4129=DIRECTION('center_axis',(0.,0.,-1.));
#4130=DIRECTION('ref_axis',(0.,1.,0.));
#4131=DIRECTION('',(0.,1.,0.));
#4132=DIRECTION('',(1.,0.,0.));
#4133=DIRECTION('',(0.,-1.,0.));
#4134=DIRECTION('center_axis',(0.,1.,-2.41352831440251E-16));
#4135=DIRECTION('ref_axis',(0.,2.41352831440251E-16,1.));
#4136=DIRECTION('',(0.,2.41352831440251E-16,1.));
#4137=DIRECTION('',(-1.,0.,0.));
#4138=DIRECTION('',(0.,-2.41352831440251E-16,-1.));
#4139=DIRECTION('center_axis',(0.,0.,1.));
#4140=DIRECTION('ref_axis',(0.,-1.,0.));
#4141=DIRECTION('',(0.,-1.,0.));
#4142=DIRECTION('',(1.,0.,0.));
#4143=DIRECTION('',(0.,1.,0.));
#4144=DIRECTION('',(1.,0.,0.));
#4145=DIRECTION('center_axis',(0.,-1.,0.));
#4146=DIRECTION('ref_axis',(0.,0.,-1.));
#4147=DIRECTION('',(0.,0.,-1.));
#4148=DIRECTION('',(1.,0.,0.));
#4149=DIRECTION('',(0.,0.,1.));
#4150=DIRECTION('center_axis',(0.,0.,1.));
#4151=DIRECTION('ref_axis',(0.,-1.,0.));
#4152=DIRECTION('',(0.,-1.,0.));
#4153=DIRECTION('',(1.,0.,0.));
#4154=DIRECTION('',(0.,1.,0.));
#4155=DIRECTION('center_axis',(0.,0.707106781186548,0.707106781186548));
#4156=DIRECTION('ref_axis',(0.,-0.707106781186548,0.707106781186548));
#4157=DIRECTION('',(0.,-0.707106781186548,0.707106781186548));
#4158=DIRECTION('',(1.,0.,0.));
#4159=DIRECTION('',(0.,0.707106781186548,-0.707106781186548));
#4160=DIRECTION('center_axis',(0.,1.,0.));
#4161=DIRECTION('ref_axis',(0.,0.,1.));
#4162=DIRECTION('',(0.,0.,1.));
#4163=DIRECTION('',(1.,0.,0.));
#4164=DIRECTION('',(0.,0.,-1.));
#4165=DIRECTION('center_axis',(0.,0.707106781186548,-0.707106781186547));
#4166=DIRECTION('ref_axis',(0.,0.707106781186547,0.707106781186548));
#4167=DIRECTION('',(0.,0.707106781186547,0.707106781186548));
#4168=DIRECTION('',(1.,0.,0.));
#4169=DIRECTION('',(0.,-0.707106781186547,-0.707106781186548));
#4170=DIRECTION('center_axis',(0.,-7.40148683083438E-16,-1.));
#4171=DIRECTION('ref_axis',(0.,1.,-7.40148683083438E-16));
#4172=DIRECTION('',(0.,1.,-7.40148683083438E-16));
#4173=DIRECTION('',(1.,0.,0.));
#4174=DIRECTION('',(0.,-1.,7.40148683083438E-16));
#4175=DIRECTION('center_axis',(0.,-1.,0.));
#4176=DIRECTION('ref_axis',(0.,0.,-1.));
#4177=DIRECTION('',(0.,0.,-1.));
#4178=DIRECTION('',(1.,0.,0.));
#4179=DIRECTION('',(0.,0.,1.));
#4180=DIRECTION('center_axis',(0.,0.,-1.));
#4181=DIRECTION('ref_axis',(0.,1.,0.));
#4182=DIRECTION('',(0.,1.,0.));
#4183=DIRECTION('',(-1.,0.,0.));
#4184=DIRECTION('',(0.,-1.,0.));
#4185=DIRECTION('center_axis',(0.,1.,0.));
#4186=DIRECTION('ref_axis',(0.,0.,1.));
#4187=DIRECTION('',(0.,0.,1.));
#4188=DIRECTION('',(1.,0.,0.));
#4189=DIRECTION('',(0.,0.,-1.));
#4190=DIRECTION('',(1.,0.,0.));
#4191=DIRECTION('center_axis',(0.,0.,1.));
#4192=DIRECTION('ref_axis',(0.,-1.,0.));
#4193=DIRECTION('',(0.,-1.,0.));
#4194=DIRECTION('',(1.,0.,0.));
#4195=DIRECTION('',(0.,1.,0.));
#4196=DIRECTION('center_axis',(0.,1.,0.));
#4197=DIRECTION('ref_axis',(0.,0.,1.));
#4198=DIRECTION('',(0.,0.,1.));
#4199=DIRECTION('',(1.,0.,0.));
#4200=DIRECTION('',(0.,0.,-1.));
#4201=DIRECTION('center_axis',(0.,0.707106781186547,-0.707106781186548));
#4202=DIRECTION('ref_axis',(0.,0.707106781186548,0.707106781186547));
#4203=DIRECTION('',(0.,0.707106781186548,0.707106781186547));
#4204=DIRECTION('',(1.,0.,0.));
#4205=DIRECTION('',(0.,-0.707106781186548,-0.707106781186547));
#4206=DIRECTION('center_axis',(0.,0.,-1.));
#4207=DIRECTION('ref_axis',(0.,1.,0.));
#4208=DIRECTION('',(0.,1.,0.));
#4209=DIRECTION('',(1.,0.,0.));
#4210=DIRECTION('',(0.,-1.,0.));
#4211=DIRECTION('center_axis',(0.,-0.707106781186547,-0.707106781186548));
#4212=DIRECTION('ref_axis',(0.,0.707106781186548,-0.707106781186547));
#4213=DIRECTION('',(0.,0.707106781186548,-0.707106781186547));
#4214=DIRECTION('',(1.,0.,0.));
#4215=DIRECTION('',(0.,-0.707106781186548,0.707106781186547));
#4216=DIRECTION('center_axis',(0.,-1.,0.));
#4217=DIRECTION('ref_axis',(0.,0.,-1.));
#4218=DIRECTION('',(0.,0.,-1.));
#4219=DIRECTION('',(1.,0.,0.));
#4220=DIRECTION('',(0.,0.,1.));
#4221=DIRECTION('center_axis',(0.,0.,1.));
#4222=DIRECTION('ref_axis',(0.,-1.,0.));
#4223=DIRECTION('',(0.,-1.,0.));
#4224=DIRECTION('',(1.,0.,0.));
#4225=DIRECTION('',(0.,1.,0.));
#4226=DIRECTION('center_axis',(0.,-1.,0.));
#4227=DIRECTION('ref_axis',(0.,0.,-1.));
#4228=DIRECTION('',(0.,0.,-1.));
#4229=DIRECTION('',(-1.,0.,0.));
#4230=DIRECTION('',(0.,0.,1.));
#4231=DIRECTION('center_axis',(1.,0.,0.));
#4232=DIRECTION('ref_axis',(0.,0.,-1.));
#4233=DIRECTION('center_axis',(1.,0.,0.));
#4234=DIRECTION('ref_axis',(0.,0.,-1.));
#4235=DIRECTION('',(1.,0.,0.));
#4236=DIRECTION('center_axis',(-1.,0.,0.));
#4237=DIRECTION('ref_axis',(0.,0.,-1.));
#4238=DIRECTION('center_axis',(0.,1.,0.));
#4239=DIRECTION('ref_axis',(0.,0.,1.));
#4240=DIRECTION('',(0.,0.,1.));
#4241=DIRECTION('',(1.,0.,0.));
#4242=DIRECTION('',(0.,0.,1.));
#4243=DIRECTION('center_axis',(0.,1.,0.));
#4244=DIRECTION('ref_axis',(0.,0.,1.));
#4245=DIRECTION('',(0.,0.,1.));
#4246=DIRECTION('',(1.,0.,0.));
#4247=DIRECTION('',(0.,0.,1.));
#4248=DIRECTION('center_axis',(0.,0.,-1.));
#4249=DIRECTION('ref_axis',(0.,1.,0.));
#4250=DIRECTION('',(0.,1.,0.));
#4251=DIRECTION('',(0.,1.,0.));
#4252=DIRECTION('center_axis',(0.,0.,-1.));
#4253=DIRECTION('ref_axis',(0.,1.,0.));
#4254=DIRECTION('',(0.,1.,0.));
#4255=DIRECTION('',(1.,0.,0.));
#4256=DIRECTION('',(0.,1.,0.));
#4257=DIRECTION('center_axis',(0.,-1.,0.));
#4258=DIRECTION('ref_axis',(0.,0.,-1.));
#4259=DIRECTION('',(0.,0.,-1.));
#4260=DIRECTION('',(0.,0.,-1.));
#4261=DIRECTION('center_axis',(0.,-1.,0.));
#4262=DIRECTION('ref_axis',(0.,0.,-1.));
#4263=DIRECTION('',(0.,0.,-1.));
#4264=DIRECTION('',(1.,0.,0.));
#4265=DIRECTION('',(0.,0.,-1.));
#4266=DIRECTION('center_axis',(0.,0.,1.));
#4267=DIRECTION('ref_axis',(0.,-1.,0.));
#4268=DIRECTION('',(0.,-1.,0.));
#4269=DIRECTION('',(0.,-1.,0.));
#4270=DIRECTION('center_axis',(0.,0.,1.));
#4271=DIRECTION('ref_axis',(0.,-1.,0.));
#4272=DIRECTION('',(0.,-1.,0.));
#4273=DIRECTION('',(0.,-1.,0.));
#4274=DIRECTION('center_axis',(1.,0.,0.));
#4275=DIRECTION('ref_axis',(0.,0.,-1.));
#4276=DIRECTION('center_axis',(1.,0.,0.));
#4277=DIRECTION('ref_axis',(0.,0.,-1.));
#4278=DIRECTION('axis',(0.,0.,1.));
#4279=DIRECTION('refdir',(1.,0.,0.));
#4280=DIRECTION('center_axis',(0.,-1.,0.));
#4281=DIRECTION('ref_axis',(1.,0.,0.));
#4282=DIRECTION('center_axis',(0.,1.,0.));
#4283=DIRECTION('ref_axis',(1.,0.,0.));
#4284=DIRECTION('',(0.,1.,0.));
#4285=DIRECTION('center_axis',(0.,-1.,0.));
#4286=DIRECTION('ref_axis',(1.,0.,0.));
#4287=DIRECTION('center_axis',(0.,1.,0.));
#4288=DIRECTION('ref_axis',(1.,0.,0.));
#4289=DIRECTION('center_axis',(0.,-1.,0.));
#4290=DIRECTION('ref_axis',(1.,0.,0.));
#4291=DIRECTION('',(-0.707106781186549,0.707106781186546,-8.65956056235496E-17));
#4292=DIRECTION('center_axis',(0.,-1.,0.));
#4293=DIRECTION('ref_axis',(0.,0.,-1.));
#4294=DIRECTION('center_axis',(0.,-1.,0.));
#4295=DIRECTION('ref_axis',(1.,0.,0.));
#4296=DIRECTION('center_axis',(0.,1.,0.));
#4297=DIRECTION('ref_axis',(1.,0.,0.));
#4298=DIRECTION('',(-0.866025403784439,-0.5,-1.06057523872491E-16));
#4299=DIRECTION('center_axis',(1.4792020664489E-16,0.,-1.));
#4300=DIRECTION('ref_axis',(-1.,0.,-1.4792020664489E-16));
#4301=DIRECTION('',(0.,1.,0.));
#4302=DIRECTION('',(-1.,0.,-1.4792020664489E-16));
#4303=DIRECTION('',(0.,1.,0.));
#4304=DIRECTION('center_axis',(0.866025403784439,0.,-0.5));
#4305=DIRECTION('ref_axis',(-0.5,0.,-0.866025403784439));
#4306=DIRECTION('',(0.,1.,0.));
#4307=DIRECTION('',(-0.5,0.,-0.866025403784439));
#4308=DIRECTION('center_axis',(0.866025403784439,0.,0.5));
#4309=DIRECTION('ref_axis',(0.5,0.,-0.866025403784439));
#4310=DIRECTION('',(0.,1.,0.));
#4311=DIRECTION('',(0.5,0.,-0.866025403784439));
#4312=DIRECTION('center_axis',(-2.95840413289779E-16,0.,1.));
#4313=DIRECTION('ref_axis',(1.,0.,2.95840413289779E-16));
#4314=DIRECTION('',(0.,1.,0.));
#4315=DIRECTION('',(1.,0.,2.95840413289779E-16));
#4316=DIRECTION('center_axis',(-0.866025403784439,0.,0.5));
#4317=DIRECTION('ref_axis',(0.5,0.,0.866025403784439));
#4318=DIRECTION('',(0.,1.,0.));
#4319=DIRECTION('',(0.5,0.,0.866025403784439));
#4320=DIRECTION('center_axis',(-0.866025403784439,0.,-0.5));
#4321=DIRECTION('ref_axis',(-0.5,0.,0.866025403784439));
#4322=DIRECTION('',(-0.5,0.,0.866025403784439));
#4323=DIRECTION('center_axis',(0.,1.,0.));
#4324=DIRECTION('ref_axis',(0.,0.,1.));
#4325=DIRECTION('center_axis',(0.,1.,0.));
#4326=DIRECTION('ref_axis',(1.,0.,0.));
#4327=DIRECTION('axis',(0.,0.,1.));
#4328=DIRECTION('refdir',(1.,0.,0.));
#4329=DIRECTION('axis',(0.,0.,1.));
#4330=DIRECTION('refdir',(1.,0.,0.));
#4331=DIRECTION('center_axis',(0.,0.,1.));
#4332=DIRECTION('ref_axis',(1.,0.,0.));
#4333=DIRECTION('center_axis',(0.,0.,1.));
#4334=DIRECTION('ref_axis',(1.,0.,0.));
#4335=DIRECTION('',(0.,0.,1.));
#4336=DIRECTION('center_axis',(0.,0.,-1.));
#4337=DIRECTION('ref_axis',(1.,0.,0.));
#4338=DIRECTION('center_axis',(0.,0.,1.));
#4339=DIRECTION('ref_axis',(1.,0.,0.));
#4340=DIRECTION('center_axis',(0.,0.,1.));
#4341=DIRECTION('ref_axis',(1.,0.,0.));
#4342=DIRECTION('',(0.,0.,1.));
#4343=DIRECTION('center_axis',(0.,0.,-1.));
#4344=DIRECTION('ref_axis',(1.,0.,0.));
#4345=DIRECTION('center_axis',(0.,0.,1.));
#4346=DIRECTION('ref_axis',(1.,0.,0.));
#4347=DIRECTION('center_axis',(0.,0.,1.));
#4348=DIRECTION('ref_axis',(1.,0.,0.));
#4349=DIRECTION('center_axis',(0.,0.,1.));
#4350=DIRECTION('ref_axis',(1.,0.,0.));
#4351=DIRECTION('',(1.,0.,0.));
#4352=DIRECTION('',(0.,1.,0.));
#4353=DIRECTION('',(-1.,0.,0.));
#4354=DIRECTION('center_axis',(0.,0.,-1.));
#4355=DIRECTION('ref_axis',(1.,0.,0.));
#4356=DIRECTION('center_axis',(0.,1.,0.));
#4357=DIRECTION('ref_axis',(-1.,0.,0.));
#4358=DIRECTION('',(0.,0.,-1.));
#4359=DIRECTION('',(0.,0.,1.));
#4360=DIRECTION('',(-1.,0.,0.));
#4361=DIRECTION('center_axis',(1.,0.,0.));
#4362=DIRECTION('ref_axis',(0.,1.,0.));
#4363=DIRECTION('',(0.,1.,0.));
#4364=DIRECTION('',(0.,0.,1.));
#4365=DIRECTION('center_axis',(0.,-1.,0.));
#4366=DIRECTION('ref_axis',(1.,0.,0.));
#4367=DIRECTION('',(0.,0.,1.));
#4368=DIRECTION('',(1.,0.,0.));
#4369=DIRECTION('center_axis',(0.,0.,1.));
#4370=DIRECTION('ref_axis',(1.,0.,0.));
#4371=DIRECTION('center_axis',(0.,0.,-1.));
#4372=DIRECTION('ref_axis',(1.,0.,0.));
#4373=DIRECTION('center_axis',(0.,0.,1.));
#4374=DIRECTION('ref_axis',(1.,0.,0.));
#4375=DIRECTION('',(0.,0.,-1.));
#4376=DIRECTION('center_axis',(0.,0.,1.));
#4377=DIRECTION('ref_axis',(1.,0.,0.));
#4378=DIRECTION('center_axis',(0.,0.,1.));
#4379=DIRECTION('ref_axis',(1.,0.,0.));
#4380=DIRECTION('',(0.,0.,-1.));
#4381=DIRECTION('center_axis',(0.,0.,-1.));
#4382=DIRECTION('ref_axis',(1.,0.,0.));
#4383=DIRECTION('center_axis',(0.,0.,1.));
#4384=DIRECTION('ref_axis',(1.,0.,0.));
#4385=DIRECTION('axis',(0.,0.,1.));
#4386=DIRECTION('refdir',(1.,0.,0.));
#4387=DIRECTION('center_axis',(0.,0.,1.));
#4388=DIRECTION('ref_axis',(1.,0.,0.));
#4389=DIRECTION('center_axis',(0.,0.,1.));
#4390=DIRECTION('ref_axis',(1.,0.,0.));
#4391=DIRECTION('',(0.,0.,1.));
#4392=DIRECTION('center_axis',(0.,0.,-1.));
#4393=DIRECTION('ref_axis',(1.,0.,0.));
#4394=DIRECTION('center_axis',(0.,0.,1.));
#4395=DIRECTION('ref_axis',(1.,0.,0.));
#4396=DIRECTION('center_axis',(0.,0.,1.));
#4397=DIRECTION('ref_axis',(1.,0.,0.));
#4398=DIRECTION('center_axis',(0.,0.,1.));
#4399=DIRECTION('ref_axis',(1.,0.,0.));
#4400=DIRECTION('center_axis',(0.,0.,1.));
#4401=DIRECTION('ref_axis',(1.,0.,0.));
#4402=DIRECTION('',(0.,0.,1.));
#4403=DIRECTION('center_axis',(0.,0.,-1.));
#4404=DIRECTION('ref_axis',(1.,0.,0.));
#4405=DIRECTION('center_axis',(0.,0.,1.));
#4406=DIRECTION('ref_axis',(1.,0.,0.));
#4407=DIRECTION('center_axis',(0.,0.,1.));
#4408=DIRECTION('ref_axis',(1.,0.,0.));
#4409=DIRECTION('center_axis',(0.,0.,1.));
#4410=DIRECTION('ref_axis',(1.,0.,0.));
#4411=DIRECTION('center_axis',(0.,0.,1.));
#4412=DIRECTION('ref_axis',(1.,0.,0.));
#4413=DIRECTION('',(0.,0.,1.));
#4414=DIRECTION('center_axis',(0.,0.,1.));
#4415=DIRECTION('ref_axis',(1.,0.,0.));
#4416=DIRECTION('center_axis',(0.,0.,1.));
#4417=DIRECTION('ref_axis',(1.,0.,0.));
#4418=DIRECTION('',(0.,0.,1.));
#4419=DIRECTION('center_axis',(0.,1.,0.));
#4420=DIRECTION('ref_axis',(-1.,0.,0.));
#4421=DIRECTION('',(-1.,0.,0.));
#4422=DIRECTION('',(0.,0.,1.));
#4423=DIRECTION('',(-1.,0.,0.));
#4424=DIRECTION('',(0.,0.,1.));
#4425=DIRECTION('center_axis',(1.,0.,0.));
#4426=DIRECTION('ref_axis',(0.,1.,0.));
#4427=DIRECTION('',(0.,1.,0.));
#4428=DIRECTION('',(0.,1.,0.));
#4429=DIRECTION('',(0.,0.,1.));
#4430=DIRECTION('center_axis',(0.,-1.,0.));
#4431=DIRECTION('ref_axis',(1.,0.,0.));
#4432=DIRECTION('',(1.,0.,0.));
#4433=DIRECTION('',(1.,0.,0.));
#4434=DIRECTION('',(0.,0.,1.));
#4435=DIRECTION('center_axis',(-1.,0.,0.));
#4436=DIRECTION('ref_axis',(0.,-1.,0.));
#4437=DIRECTION('',(0.,-1.,0.));
#4438=DIRECTION('',(0.,-1.,0.));
#4439=DIRECTION('center_axis',(0.,0.,1.));
#4440=DIRECTION('ref_axis',(1.,0.,0.));
#4441=DIRECTION('center_axis',(0.,0.,1.));
#4442=DIRECTION('ref_axis',(1.,0.,0.));
#4443=DIRECTION('axis',(0.,0.,1.));
#4444=DIRECTION('refdir',(1.,0.,0.));
#4445=DIRECTION('center_axis',(0.,1.,0.));
#4446=DIRECTION('ref_axis',(0.,0.,1.));
#4447=DIRECTION('center_axis',(0.,-1.,0.));
#4448=DIRECTION('ref_axis',(1.,0.,0.));
#4449=DIRECTION('center_axis',(0.,-1.,0.));
#4450=DIRECTION('ref_axis',(1.,0.,0.));
#4451=DIRECTION('center_axis',(0.,-1.,0.));
#4452=DIRECTION('ref_axis',(1.,0.,0.));
#4453=DIRECTION('',(0.707106781186547,0.707106781186548,8.65956056235493E-17));
#4454=DIRECTION('center_axis',(0.,-1.,0.));
#4455=DIRECTION('ref_axis',(1.,0.,0.));
#4456=DIRECTION('center_axis',(0.,-1.,0.));
#4457=DIRECTION('ref_axis',(1.,0.,0.));
#4458=DIRECTION('',(0.,1.,0.));
#4459=DIRECTION('center_axis',(0.,1.,0.));
#4460=DIRECTION('ref_axis',(1.,0.,0.));
#4461=DIRECTION('center_axis',(0.,-1.,0.));
#4462=DIRECTION('ref_axis',(1.,0.,0.));
#4463=DIRECTION('',(-0.707106781186547,0.707106781186548,-8.65956056235493E-17));
#4464=DIRECTION('center_axis',(0.,-1.,0.));
#4465=DIRECTION('ref_axis',(0.,0.,-1.));
#4466=DIRECTION('center_axis',(0.,-1.,0.));
#4467=DIRECTION('ref_axis',(1.,0.,0.));
#4468=DIRECTION('center_axis',(0.,1.,0.));
#4469=DIRECTION('ref_axis',(1.,0.,0.));
#4470=DIRECTION('center_axis',(0.,1.,0.));
#4471=DIRECTION('ref_axis',(1.,0.,0.));
#4472=DIRECTION('',(-0.447213595499958,0.894427190999916,-5.47678698264203E-17));
#4473=DIRECTION('center_axis',(0.,-1.,0.));
#4474=DIRECTION('ref_axis',(1.,0.,0.));
#4475=DIRECTION('center_axis',(0.,1.,0.));
#4476=DIRECTION('ref_axis',(1.,0.,0.));
#4477=DIRECTION('',(0.,1.,0.));
#4478=DIRECTION('center_axis',(0.,1.,0.));
#4479=DIRECTION('ref_axis',(1.,0.,0.));
#4480=DIRECTION('center_axis',(0.,-1.,0.));
#4481=DIRECTION('ref_axis',(1.,0.,0.));
#4482=DIRECTION('',(-0.707106781186547,0.707106781186548,-8.65956056235493E-17));
#4483=DIRECTION('center_axis',(0.,-1.,0.));
#4484=DIRECTION('ref_axis',(0.,0.,-1.));
#4485=DIRECTION('center_axis',(0.866025403784439,0.,-0.5));
#4486=DIRECTION('ref_axis',(0.5,0.,0.866025403784439));
#4487=DIRECTION('',(-0.5,0.,-0.866025403784439));
#4488=DIRECTION('',(0.,-1.,0.));
#4489=DIRECTION('',(0.5,0.,0.866025403784439));
#4490=DIRECTION('',(0.,-1.,0.));
#4491=DIRECTION('center_axis',(1.60246890531964E-16,0.,-1.));
#4492=DIRECTION('ref_axis',(1.,0.,1.60246890531964E-16));
#4493=DIRECTION('',(-1.,0.,-1.60246890531964E-16));
#4494=DIRECTION('',(0.,-1.,0.));
#4495=DIRECTION('',(1.,0.,1.60246890531964E-16));
#4496=DIRECTION('center_axis',(-0.866025403784439,0.,-0.5));
#4497=DIRECTION('ref_axis',(0.5,0.,-0.866025403784439));
#4498=DIRECTION('',(-0.5,0.,0.866025403784439));
#4499=DIRECTION('',(0.,-1.,0.));
#4500=DIRECTION('',(0.5,0.,-0.866025403784439));
#4501=DIRECTION('center_axis',(-0.866025403784439,0.,0.5));
#4502=DIRECTION('ref_axis',(-0.5,0.,-0.866025403784439));
#4503=DIRECTION('',(0.5,0.,0.866025403784439));
#4504=DIRECTION('',(0.,-1.,0.));
#4505=DIRECTION('',(-0.5,0.,-0.866025403784439));
#4506=DIRECTION('center_axis',(-1.60246890531964E-16,0.,1.));
#4507=DIRECTION('ref_axis',(-1.,0.,-1.60246890531964E-16));
#4508=DIRECTION('',(1.,0.,1.60246890531964E-16));
#4509=DIRECTION('',(0.,-1.,0.));
#4510=DIRECTION('',(-1.,0.,-1.60246890531964E-16));
#4511=DIRECTION('center_axis',(0.866025403784439,0.,0.5));
#4512=DIRECTION('ref_axis',(-0.5,0.,0.866025403784439));
#4513=DIRECTION('',(0.5,0.,-0.866025403784439));
#4514=DIRECTION('',(-0.5,0.,0.866025403784439));
#4515=DIRECTION('center_axis',(0.,1.,0.));
#4516=DIRECTION('ref_axis',(1.,0.,0.));
#4517=DIRECTION('center_axis',(0.,-1.,0.));
#4518=DIRECTION('ref_axis',(0.,0.,-1.));
#4519=DIRECTION('axis',(0.,0.,1.));
#4520=DIRECTION('refdir',(1.,0.,0.));
#4521=DIRECTION('center_axis',(0.,1.,0.));
#4522=DIRECTION('ref_axis',(1.,0.,0.));
#4523=DIRECTION('center_axis',(0.,-1.,0.));
#4524=DIRECTION('ref_axis',(1.,0.,0.));
#4525=DIRECTION('',(0.,-1.,0.));
#4526=DIRECTION('center_axis',(0.,-1.,0.));
#4527=DIRECTION('ref_axis',(1.,0.,0.));
#4528=DIRECTION('center_axis',(0.,1.,0.));
#4529=DIRECTION('ref_axis',(1.,0.,0.));
#4530=DIRECTION('center_axis',(0.,1.,0.));
#4531=DIRECTION('ref_axis',(1.,0.,0.));
#4532=DIRECTION('',(0.,-1.,0.));
#4533=DIRECTION('center_axis',(0.,1.,0.));
#4534=DIRECTION('ref_axis',(1.,0.,0.));
#4535=DIRECTION('center_axis',(0.,1.,0.));
#4536=DIRECTION('ref_axis',(1.,0.,0.));
#4537=DIRECTION('center_axis',(0.,1.,0.));
#4538=DIRECTION('ref_axis',(1.,0.,0.));
#4539=DIRECTION('',(0.,0.,1.));
#4540=DIRECTION('',(1.,0.,0.));
#4541=DIRECTION('',(0.,0.,1.));
#4542=DIRECTION('',(1.,0.,0.));
#4543=DIRECTION('',(0.,-1.,2.22044604925031E-16));
#4544=DIRECTION('',(1.,0.,0.));
#4545=DIRECTION('',(0.,-1.,2.22044604925031E-16));
#4546=DIRECTION('',(1.,0.,0.));
#4547=DIRECTION('',(0.,0.,1.));
#4548=DIRECTION('',(1.,0.,0.));
#4549=DIRECTION('',(0.,-1.,2.22044604925031E-16));
#4550=DIRECTION('',(1.,0.,0.));
#4551=DIRECTION('',(0.,-1.,2.22044604925031E-16));
#4552=DIRECTION('',(1.,0.,0.));
#4553=DIRECTION('',(0.,0.,1.));
#4554=DIRECTION('',(1.,0.,0.));
#4555=DIRECTION('',(0.,-1.,2.22044604925031E-16));
#4556=DIRECTION('',(1.,0.,0.));
#4557=DIRECTION('',(0.,1.,2.22044604925031E-16));
#4558=DIRECTION('',(1.,0.,0.));
#4559=DIRECTION('axis',(0.,0.,1.));
#4560=DIRECTION('refdir',(1.,0.,0.));
#4561=DIRECTION('center_axis',(0.,1.,0.));
#4562=DIRECTION('ref_axis',(1.,0.,0.));
#4563=DIRECTION('',(0.866025403784439,-0.5,1.06057523872491E-16));
#4564=DIRECTION('center_axis',(0.,-1.,0.));
#4565=DIRECTION('ref_axis',(1.,0.,0.));
#4566=DIRECTION('center_axis',(0.,-1.,0.));
#4567=DIRECTION('ref_axis',(1.,0.,0.));
#4568=DIRECTION('center_axis',(0.,1.,0.));
#4569=DIRECTION('ref_axis',(1.,0.,0.));
#4570=DIRECTION('',(-0.866025403784439,-0.5,-1.06057523872491E-16));
#4571=DIRECTION('center_axis',(1.4792020664489E-16,0.,-1.));
#4572=DIRECTION('ref_axis',(-1.,0.,-1.4792020664489E-16));
#4573=DIRECTION('',(0.,1.,0.));
#4574=DIRECTION('',(0.,1.,0.));
#4575=DIRECTION('center_axis',(-0.866025403784439,0.,-0.5));
#4576=DIRECTION('ref_axis',(-0.5,0.,0.866025403784439));
#4577=DIRECTION('',(0.,1.,0.));
#4578=DIRECTION('center_axis',(-0.866025403784439,0.,0.5));
#4579=DIRECTION('ref_axis',(0.5,0.,0.866025403784439));
#4580=DIRECTION('',(0.,1.,0.));
#4581=DIRECTION('center_axis',(0.,1.,0.));
#4582=DIRECTION('ref_axis',(1.,0.,0.));
#4583=DIRECTION('center_axis',(0.,1.,0.));
#4584=DIRECTION('ref_axis',(1.,0.,0.));
#4585=DIRECTION('',(0.,-1.,0.));
#4586=DIRECTION('center_axis',(0.,1.,0.));
#4587=DIRECTION('ref_axis',(1.,0.,0.));
#4588=DIRECTION('center_axis',(-2.95840413289779E-16,0.,1.));
#4589=DIRECTION('ref_axis',(1.,0.,2.95840413289779E-16));
#4590=DIRECTION('',(0.,1.,0.));
#4591=DIRECTION('center_axis',(0.866025403784439,0.,-0.5));
#4592=DIRECTION('ref_axis',(-0.5,0.,-0.866025403784439));
#4593=DIRECTION('',(0.,1.,0.));
#4594=DIRECTION('center_axis',(0.866025403784439,0.,0.5));
#4595=DIRECTION('ref_axis',(0.5,0.,-0.866025403784439));
#4596=DIRECTION('center_axis',(0.,1.,0.));
#4597=DIRECTION('ref_axis',(1.,0.,0.));
#4598=DIRECTION('center_axis',(0.,1.,0.));
#4599=DIRECTION('ref_axis',(1.,0.,0.));
#4600=DIRECTION('axis',(0.,0.,1.));
#4601=DIRECTION('refdir',(1.,0.,0.));
#4602=DIRECTION('center_axis',(0.,0.,1.));
#4603=DIRECTION('ref_axis',(1.,0.,0.));
#4604=DIRECTION('',(0.,0.,-1.));
#4605=DIRECTION('center_axis',(0.,0.,-1.));
#4606=DIRECTION('ref_axis',(1.,0.,0.));
#4607=DIRECTION('',(0.,0.,1.));
#4608=DIRECTION('center_axis',(0.,0.,1.));
#4609=DIRECTION('ref_axis',(1.,0.,0.));
#4610=DIRECTION('center_axis',(0.,0.,1.));
#4611=DIRECTION('ref_axis',(-1.,-1.22464679914735E-16,0.));
#4612=DIRECTION('',(0.,0.,1.));
#4613=DIRECTION('center_axis',(0.,0.,1.));
#4614=DIRECTION('ref_axis',(1.,0.,0.));
#4615=DIRECTION('',(0.,0.,-1.));
#4616=DIRECTION('center_axis',(0.,0.,-1.));
#4617=DIRECTION('ref_axis',(1.,0.,0.));
#4618=DIRECTION('center_axis',(0.,0.,1.));
#4619=DIRECTION('ref_axis',(1.,0.,0.));
#4620=DIRECTION('',(0.,0.,-1.));
#4621=DIRECTION('center_axis',(0.,0.,-1.));
#4622=DIRECTION('ref_axis',(1.,0.,0.));
#4623=DIRECTION('',(0.,0.,1.));
#4624=DIRECTION('center_axis',(0.,0.,1.));
#4625=DIRECTION('ref_axis',(1.,0.,0.));
#4626=DIRECTION('center_axis',(0.,0.,1.));
#4627=DIRECTION('ref_axis',(1.,0.,0.));
#4628=DIRECTION('',(0.,0.,-1.));
#4629=DIRECTION('center_axis',(0.,0.,-1.));
#4630=DIRECTION('ref_axis',(1.,0.,0.));
#4631=DIRECTION('',(0.,0.,1.));
#4632=DIRECTION('center_axis',(0.,0.,1.));
#4633=DIRECTION('ref_axis',(1.,0.,0.));
#4634=DIRECTION('center_axis',(0.,0.,1.));
#4635=DIRECTION('ref_axis',(1.,0.,0.));
#4636=DIRECTION('',(0.,0.,-1.));
#4637=DIRECTION('center_axis',(0.,0.,-1.));
#4638=DIRECTION('ref_axis',(1.,0.,0.));
#4639=DIRECTION('',(0.,0.,1.));
#4640=DIRECTION('center_axis',(0.,0.,1.));
#4641=DIRECTION('ref_axis',(1.,0.,0.));
#4642=DIRECTION('center_axis',(0.,0.,1.));
#4643=DIRECTION('ref_axis',(1.,0.,0.));
#4644=DIRECTION('',(0.,0.,-1.));
#4645=DIRECTION('center_axis',(0.,0.,-1.));
#4646=DIRECTION('ref_axis',(1.,0.,0.));
#4647=DIRECTION('',(0.,0.,1.));
#4648=DIRECTION('center_axis',(0.,0.,1.));
#4649=DIRECTION('ref_axis',(1.,0.,0.));
#4650=DIRECTION('center_axis',(0.,0.,1.));
#4651=DIRECTION('ref_axis',(1.,0.,0.));
#4652=DIRECTION('center_axis',(0.,0.,1.));
#4653=DIRECTION('ref_axis',(1.,0.,0.));
#4654=DIRECTION('center_axis',(0.,0.,1.));
#4655=DIRECTION('ref_axis',(1.,0.,0.));
#4656=DIRECTION('center_axis',(0.,0.,1.));
#4657=DIRECTION('ref_axis',(1.,0.,0.));
#4658=DIRECTION('center_axis',(0.,0.,1.));
#4659=DIRECTION('ref_axis',(1.,0.,0.));
#4660=DIRECTION('center_axis',(0.,0.,1.));
#4661=DIRECTION('ref_axis',(1.,0.,0.));
#4662=DIRECTION('center_axis',(0.,0.,1.));
#4663=DIRECTION('ref_axis',(1.,0.,0.));
#4664=DIRECTION('center_axis',(0.,0.,-1.));
#4665=DIRECTION('ref_axis',(1.,0.,0.));
#4666=DIRECTION('center_axis',(0.,0.,1.));
#4667=DIRECTION('ref_axis',(1.,0.,0.));
#4668=DIRECTION('center_axis',(0.,0.,1.));
#4669=DIRECTION('ref_axis',(1.,0.,0.));
#4670=DIRECTION('center_axis',(0.,0.,1.));
#4671=DIRECTION('ref_axis',(1.,0.,0.));
#4672=DIRECTION('center_axis',(0.,0.,1.));
#4673=DIRECTION('ref_axis',(1.,0.,0.));
#4674=DIRECTION('center_axis',(0.,0.,1.));
#4675=DIRECTION('ref_axis',(1.,0.,0.));
#4676=DIRECTION('center_axis',(0.,0.,1.));
#4677=DIRECTION('ref_axis',(1.,0.,0.));
#4678=DIRECTION('center_axis',(0.,0.,1.));
#4679=DIRECTION('ref_axis',(1.,0.,0.));
#4680=DIRECTION('center_axis',(0.,0.,1.));
#4681=DIRECTION('ref_axis',(1.,0.,0.));
#4682=DIRECTION('center_axis',(0.,0.,1.));
#4683=DIRECTION('ref_axis',(1.,0.,0.));
#4684=DIRECTION('center_axis',(0.,0.,1.));
#4685=DIRECTION('ref_axis',(1.,0.,0.));
#4686=DIRECTION('center_axis',(0.,0.,1.));
#4687=DIRECTION('ref_axis',(1.,0.,0.));
#4688=DIRECTION('center_axis',(0.,0.,1.));
#4689=DIRECTION('ref_axis',(1.,0.,0.));
#4690=DIRECTION('center_axis',(0.,1.,0.));
#4691=DIRECTION('ref_axis',(-1.,0.,0.));
#4692=DIRECTION('',(-1.,0.,0.));
#4693=DIRECTION('',(0.,0.,1.));
#4694=DIRECTION('',(-1.,0.,0.));
#4695=DIRECTION('',(0.,0.,1.));
#4696=DIRECTION('center_axis',(-0.866025403784438,0.500000000000001,0.));
#4697=DIRECTION('ref_axis',(-0.500000000000001,-0.866025403784438,0.));
#4698=DIRECTION('',(-0.500000000000001,-0.866025403784438,0.));
#4699=DIRECTION('',(-0.500000000000001,-0.866025403784438,0.));
#4700=DIRECTION('',(0.,0.,1.));
#4701=DIRECTION('center_axis',(-0.866025403784439,-0.5,0.));
#4702=DIRECTION('ref_axis',(0.5,-0.866025403784439,0.));
#4703=DIRECTION('',(0.5,-0.866025403784439,0.));
#4704=DIRECTION('',(0.5,-0.866025403784439,0.));
#4705=DIRECTION('',(0.,0.,1.));
#4706=DIRECTION('center_axis',(0.,-1.,0.));
#4707=DIRECTION('ref_axis',(1.,0.,0.));
#4708=DIRECTION('',(1.,0.,0.));
#4709=DIRECTION('',(1.,0.,0.));
#4710=DIRECTION('',(0.,0.,1.));
#4711=DIRECTION('center_axis',(0.866025403784439,0.5,0.));
#4712=DIRECTION('ref_axis',(-0.5,0.866025403784439,0.));
#4713=DIRECTION('',(-0.5,0.866025403784439,0.));
#4714=DIRECTION('',(0.,0.,1.));
#4715=DIRECTION('',(-0.5,0.866025403784439,0.));
#4716=DIRECTION('center_axis',(0.866025403784439,-0.5,0.));
#4717=DIRECTION('ref_axis',(0.5,0.866025403784439,0.));
#4718=DIRECTION('',(0.5,0.866025403784439,0.));
#4719=DIRECTION('',(0.5,0.866025403784439,0.));
#4720=DIRECTION('center_axis',(0.,0.,1.));
#4721=DIRECTION('ref_axis',(1.,0.,0.));
#4722=DIRECTION('center_axis',(0.,0.,-1.));
#4723=DIRECTION('ref_axis',(1.,0.,0.));
#4724=DIRECTION('center_axis',(0.,0.,1.));
#4725=DIRECTION('ref_axis',(1.,0.,0.));
#4726=DIRECTION('',(0.,0.,-1.));
#4727=DIRECTION('center_axis',(0.,0.,1.));
#4728=DIRECTION('ref_axis',(1.,0.,0.));
#4729=DIRECTION('',(0.,0.,1.));
#4730=DIRECTION('',(1.,0.,0.));
#4731=DIRECTION('',(0.,0.,1.));
#4732=DIRECTION('',(1.,0.,0.));
#4733=DIRECTION('',(0.,-1.,2.22044604925031E-16));
#4734=DIRECTION('',(1.,0.,0.));
#4735=DIRECTION('',(0.,-1.,2.22044604925031E-16));
#4736=DIRECTION('',(1.,0.,0.));
#4737=DIRECTION('',(0.,-1.,2.22044604925031E-16));
#4738=DIRECTION('',(1.,0.,0.));
#4739=DIRECTION('',(0.,-1.,2.22044604925031E-16));
#4740=DIRECTION('',(1.,0.,0.));
#4741=DIRECTION('',(0.,0.,1.));
#4742=DIRECTION('',(1.,0.,0.));
#4743=DIRECTION('',(0.,0.,1.));
#4744=DIRECTION('',(1.,0.,0.));
#4745=DIRECTION('',(4.24122425686576E-18,6.10852803337894E-17,1.));
#4746=DIRECTION('',(0.754385960422041,0.656431125646946,-4.32977993643493E-17));
#4747=CARTESIAN_POINT('',(0.,0.,0.));
#4748=CARTESIAN_POINT('',(0.,0.,0.));
#4749=CARTESIAN_POINT('',(0.,0.,0.));
#4750=CARTESIAN_POINT('Origin',(7.5,0.,2.));
#4751=CARTESIAN_POINT('',(6.7,-9.79717439317883E-17,3.2));
#4752=CARTESIAN_POINT('Origin',(7.5,0.,3.2));
#4753=CARTESIAN_POINT('',(6.7,-9.79717439317883E-17,2.));
#4754=CARTESIAN_POINT('',(6.7,-9.79717439317883E-17,2.));
#4755=CARTESIAN_POINT('Origin',(7.5,0.,2.));
#4756=CARTESIAN_POINT('Origin',(7.5,0.,2.));
#4757=CARTESIAN_POINT('',(7.225,-3.36777869765523E-17,2.));
#4758=CARTESIAN_POINT('Origin',(7.5,0.,2.));
#4759=CARTESIAN_POINT('Origin',(2.5,0.,2.));
#4760=CARTESIAN_POINT('',(1.7,-9.79717439317882E-17,3.2));
#4761=CARTESIAN_POINT('Origin',(2.5,0.,3.2));
#4762=CARTESIAN_POINT('',(1.7,-9.79717439317882E-17,2.));
#4763=CARTESIAN_POINT('',(1.7,-9.79717439317882E-17,2.));
#4764=CARTESIAN_POINT('Origin',(2.5,0.,2.));
#4765=CARTESIAN_POINT('Origin',(2.5,0.,2.));
#4766=CARTESIAN_POINT('',(2.225,-3.36777869765522E-17,2.));
#4767=CARTESIAN_POINT('Origin',(2.5,0.,2.));
#4768=CARTESIAN_POINT('Origin',(2.5,0.,3.1));
#4769=CARTESIAN_POINT('',(2.225,3.36777869765522E-17,4.));
#4770=CARTESIAN_POINT('',(2.225,-3.36777869765522E-17,3.1));
#4771=CARTESIAN_POINT('Origin',(2.5,0.,4.));
#4772=CARTESIAN_POINT('Origin',(7.5,0.,3.1));
#4773=CARTESIAN_POINT('',(7.225,3.36777869765523E-17,4.));
#4774=CARTESIAN_POINT('',(7.225,-3.36777869765523E-17,3.1));
#4775=CARTESIAN_POINT('Origin',(7.5,0.,4.));
#4776=CARTESIAN_POINT('Origin',(5.,0.,3.1));
#4777=CARTESIAN_POINT('',(4.575,-5.20474889637625E-17,3.2));
#4778=CARTESIAN_POINT('Origin',(5.,0.,3.2));
#4779=CARTESIAN_POINT('',(4.575,5.20474889637625E-17,4.4));
#4780=CARTESIAN_POINT('',(4.575,-5.20474889637625E-17,3.1));
#4781=CARTESIAN_POINT('Origin',(5.,0.,4.4));
#4782=CARTESIAN_POINT('Origin',(5.,0.,4.));
#4783=CARTESIAN_POINT('',(3.7,-1.59204083889156E-16,4.4));
#4784=CARTESIAN_POINT('Origin',(5.,0.,4.4));
#4785=CARTESIAN_POINT('',(3.7,-1.59204083889156E-16,4.));
#4786=CARTESIAN_POINT('',(3.7,-1.59204083889156E-16,4.));
#4787=CARTESIAN_POINT('Origin',(5.,0.,4.));
#4788=CARTESIAN_POINT('Origin',(5.,0.,4.4));
#4789=CARTESIAN_POINT('Origin',(8.5,2.,3.2));
#4790=CARTESIAN_POINT('',(8.5,2.,3.2));
#4791=CARTESIAN_POINT('',(1.5,2.,3.2));
#4792=CARTESIAN_POINT('',(8.5,2.,3.2));
#4793=CARTESIAN_POINT('',(1.5,2.,4.));
#4794=CARTESIAN_POINT('',(1.5,2.,3.2));
#4795=CARTESIAN_POINT('',(8.5,2.,4.));
#4796=CARTESIAN_POINT('',(8.5,2.,4.));
#4797=CARTESIAN_POINT('',(8.5,2.,3.2));
#4798=CARTESIAN_POINT('Origin',(8.5,-2.,3.2));
#4799=CARTESIAN_POINT('',(8.5,-2.,3.2));
#4800=CARTESIAN_POINT('',(8.5,-2.,3.2));
#4801=CARTESIAN_POINT('',(8.5,-2.,4.));
#4802=CARTESIAN_POINT('',(8.5,-2.,4.));
#4803=CARTESIAN_POINT('',(8.5,-2.,3.2));
#4804=CARTESIAN_POINT('Origin',(1.5,-2.,3.2));
#4805=CARTESIAN_POINT('',(1.5,-2.,3.2));
#4806=CARTESIAN_POINT('',(1.5,-2.,3.2));
#4807=CARTESIAN_POINT('',(1.5,-2.,4.));
#4808=CARTESIAN_POINT('',(1.5,-2.,4.));
#4809=CARTESIAN_POINT('',(1.5,-2.,3.2));
#4810=CARTESIAN_POINT('Origin',(1.5,2.,3.2));
#4811=CARTESIAN_POINT('',(1.5,2.,3.2));
#4812=CARTESIAN_POINT('',(1.5,2.,4.));
#4813=CARTESIAN_POINT('Origin',(5.,0.,4.));
#4814=CARTESIAN_POINT('Origin',(5.,0.,3.2));
#4815=CARTESIAN_POINT('',(0.,0.,0.));
#4816=CARTESIAN_POINT('Origin',(0.,0.395,0.25));
#4817=CARTESIAN_POINT('',(-0.5,0.3,0.25));
#4818=CARTESIAN_POINT('',(0.5,0.3,0.25));
#4819=CARTESIAN_POINT('',(0.25,0.3,0.25));
#4820=CARTESIAN_POINT('',(-0.5,0.5,0.25));
#4821=CARTESIAN_POINT('',(-0.5,0.5,0.25));
#4822=CARTESIAN_POINT('',(0.5,0.5,0.25));
#4823=CARTESIAN_POINT('',(0.5,0.5,0.25));
#4824=CARTESIAN_POINT('',(0.5,0.29,0.25));
#4825=CARTESIAN_POINT('Origin',(0.5,0.5,0.25));
#4826=CARTESIAN_POINT('',(-0.5,0.5,0.4));
#4827=CARTESIAN_POINT('',(-0.5,0.5,0.25));
#4828=CARTESIAN_POINT('',(0.5,0.5,0.4));
#4829=CARTESIAN_POINT('',(0.5,0.5,0.4));
#4830=CARTESIAN_POINT('',(0.5,0.5,0.25));
#4831=CARTESIAN_POINT('Origin',(0.,0.,0.4));
#4832=CARTESIAN_POINT('',(-0.5,-0.5,0.4));
#4833=CARTESIAN_POINT('',(-0.5,0.5,0.4));
#4834=CARTESIAN_POINT('',(0.5,-0.5,0.4));
#4835=CARTESIAN_POINT('',(-0.5,-0.5,0.4));
#4836=CARTESIAN_POINT('',(0.5,-0.3,0.4));
#4837=CARTESIAN_POINT('',(-0.2117,2.59257727379495E-17,0.4));
#4838=CARTESIAN_POINT('Origin',(0.,0.,0.4));
#4839=CARTESIAN_POINT('Origin',(-0.5,0.3,0.));
#4840=CARTESIAN_POINT('',(-0.5,0.3,0.15));
#4841=CARTESIAN_POINT('',(-0.5,0.3,0.));
#4842=CARTESIAN_POINT('',(-0.5,0.15,0.));
#4843=CARTESIAN_POINT('',(-0.5,0.225,0.075));
#4844=CARTESIAN_POINT('',(-0.5,-0.15,0.));
#4845=CARTESIAN_POINT('',(-0.5,0.3,0.));
#4846=CARTESIAN_POINT('',(-0.5,-0.3,0.15));
#4847=CARTESIAN_POINT('',(-0.5,-0.075,-0.075));
#4848=CARTESIAN_POINT('',(-0.5,-0.3,0.25));
#4849=CARTESIAN_POINT('',(-0.5,-0.3,0.));
#4850=CARTESIAN_POINT('',(-0.5,-0.5,0.25));
#4851=CARTESIAN_POINT('',(-0.5,-0.29,0.25));
#4852=CARTESIAN_POINT('',(-0.5,-0.5,0.25));
#4853=CARTESIAN_POINT('Origin',(-0.5,-0.5,0.25));
#4854=CARTESIAN_POINT('',(0.5,-0.5,0.25));
#4855=CARTESIAN_POINT('',(-0.5,-0.5,0.25));
#4856=CARTESIAN_POINT('',(0.5,-0.5,0.25));
#4857=CARTESIAN_POINT('Origin',(0.,-0.395,0.25));
#4858=CARTESIAN_POINT('',(0.5,-0.3,0.25));
#4859=CARTESIAN_POINT('',(-0.25,-0.3,0.25));
#4860=CARTESIAN_POINT('',(0.5,-0.5,0.25));
#4861=CARTESIAN_POINT('Origin',(0.5,-0.3,0.));
#4862=CARTESIAN_POINT('',(0.5,-0.3,0.15));
#4863=CARTESIAN_POINT('',(0.5,-0.3,0.));
#4864=CARTESIAN_POINT('',(0.5,-0.15,0.));
#4865=CARTESIAN_POINT('',(0.5,-0.225,0.075));
#4866=CARTESIAN_POINT('',(0.5,0.15,0.));
#4867=CARTESIAN_POINT('',(0.5,-0.3,0.));
#4868=CARTESIAN_POINT('',(0.5,0.3,0.15));
#4869=CARTESIAN_POINT('',(0.5,0.075,-0.075));
#4870=CARTESIAN_POINT('',(0.5,0.3,0.));
#4871=CARTESIAN_POINT('Origin',(-0.5,-0.3,0.));
#4872=CARTESIAN_POINT('',(-0.25,-0.3,0.15));
#4873=CARTESIAN_POINT('Origin',(-0.25,-0.225,0.075));
#4874=CARTESIAN_POINT('',(-0.149388386429468,-0.15,0.));
#4875=CARTESIAN_POINT('',(-0.25,-0.15,0.));
#4876=CARTESIAN_POINT('',(0.149388386429468,-0.15,0.));
#4877=CARTESIAN_POINT('Origin',(0.,0.,-0.15));
#4878=CARTESIAN_POINT('',(-0.25,-0.15,0.));
#4879=CARTESIAN_POINT('Origin',(0.,0.,-0.1));
#4880=CARTESIAN_POINT('',(-0.2117,-2.59257727379495E-17,0.));
#4881=CARTESIAN_POINT('Origin',(0.,0.,0.));
#4882=CARTESIAN_POINT('',(-0.2117,-2.59257727379495E-17,-0.1));
#4883=CARTESIAN_POINT('',(-0.149388386429468,0.15,0.));
#4884=CARTESIAN_POINT('Origin',(0.,0.,0.));
#4885=CARTESIAN_POINT('',(0.149388386429468,0.15,0.));
#4886=CARTESIAN_POINT('Origin',(0.,0.,-0.15));
#4887=CARTESIAN_POINT('Origin',(0.,0.,0.));
#4888=CARTESIAN_POINT('Origin',(0.,0.,0.));
#4889=CARTESIAN_POINT('',(0.25,0.15,0.));
#4890=CARTESIAN_POINT('Origin',(0.,0.,0.));
#4891=CARTESIAN_POINT('',(0.25,0.15,0.));
#4892=CARTESIAN_POINT('Origin',(0.25,0.225,0.075));
#4893=CARTESIAN_POINT('',(0.25,0.3,0.15));
#4894=CARTESIAN_POINT('Origin',(0.5,0.3,0.));
#4895=CARTESIAN_POINT('',(0.,0.,0.));
#4896=CARTESIAN_POINT('Origin',(0.,0.09,0.));
#4897=CARTESIAN_POINT('',(-0.285,0.1,3.49024337756996E-17));
#4898=CARTESIAN_POINT('Origin',(0.,0.1,0.));
#4899=CARTESIAN_POINT('',(-0.265,0.08,-3.24531401774049E-17));
#4900=CARTESIAN_POINT('',(-0.275,0.09,3.36777869765522E-17));
#4901=CARTESIAN_POINT('Origin',(0.,0.08,0.));
#4902=CARTESIAN_POINT('Origin',(0.,0.,0.));
#4903=CARTESIAN_POINT('',(-0.265,0.,3.24531401774049E-17));
#4904=CARTESIAN_POINT('',(-0.265,0.,3.24531401774049E-17));
#4905=CARTESIAN_POINT('Origin',(0.,0.,0.));
#4906=CARTESIAN_POINT('Origin',(0.,0.1,0.));
#4907=CARTESIAN_POINT('',(-0.5,0.1,6.12323399573677E-17));
#4908=CARTESIAN_POINT('Origin',(0.,0.1,0.));
#4909=CARTESIAN_POINT('Origin',(0.,0.,0.));
#4910=CARTESIAN_POINT('',(-0.5,0.,6.12323399573677E-17));
#4911=CARTESIAN_POINT('',(-0.5,0.,6.12323399573677E-17));
#4912=CARTESIAN_POINT('Origin',(0.,0.,0.));
#4913=CARTESIAN_POINT('Origin',(0.,0.,0.));
#4914=CARTESIAN_POINT('',(0.,0.,0.));
#4915=CARTESIAN_POINT('Origin',(0.,-1.39,0.));
#4916=CARTESIAN_POINT('',(-0.25,-1.39,3.06161699786838E-17));
#4917=CARTESIAN_POINT('Origin',(0.,-1.39,0.));
#4918=CARTESIAN_POINT('',(-0.24505,-1.39,3.00099698131059E-17));
#4919=CARTESIAN_POINT('Origin',(0.,-1.39,0.));
#4920=CARTESIAN_POINT('Origin',(0.,-2.6,0.));
#4921=CARTESIAN_POINT('',(-0.25,-2.6,3.06161699786838E-17));
#4922=CARTESIAN_POINT('',(-0.25,-2.6,3.06161699786838E-17));
#4923=CARTESIAN_POINT('Origin',(0.,-2.6,0.));
#4924=CARTESIAN_POINT('Origin',(0.,-2.6,0.));
#4925=CARTESIAN_POINT('Origin',(0.375,0.5,0.));
#4926=CARTESIAN_POINT('',(-0.375,0.5,-4.59242549680257E-17));
#4927=CARTESIAN_POINT('Origin',(0.,0.5,0.));
#4928=CARTESIAN_POINT('Origin',(0.,0.475,0.));
#4929=CARTESIAN_POINT('',(-0.425,0.45,-5.20474889637625E-17));
#4930=CARTESIAN_POINT('Origin',(0.,0.45,0.));
#4931=CARTESIAN_POINT('',(-0.4,0.475,-4.89858719658941E-17));
#4932=CARTESIAN_POINT('Origin',(0.,0.24,0.));
#4933=CARTESIAN_POINT('',(-0.425,0.0299999999999998,-5.20474889637625E-17));
#4934=CARTESIAN_POINT('Origin',(0.,0.0299999999999998,0.));
#4935=CARTESIAN_POINT('',(-0.425,0.24,-5.20474889637625E-17));
#4936=CARTESIAN_POINT('Origin',(0.,0.0150000000000001,0.));
#4937=CARTESIAN_POINT('',(-0.395,4.85722573273506E-17,-4.83735485663204E-17));
#4938=CARTESIAN_POINT('Origin',(0.,0.,0.));
#4939=CARTESIAN_POINT('',(-0.41,0.0150000000000001,-5.02105187650415E-17));
#4940=CARTESIAN_POINT('Origin',(0.27,0.,0.));
#4941=CARTESIAN_POINT('',(-0.27,0.,-3.30654635769785E-17));
#4942=CARTESIAN_POINT('Origin',(0.,0.,0.));
#4943=CARTESIAN_POINT('Origin',(0.,-0.02,0.));
#4944=CARTESIAN_POINT('',(-0.24505,-0.0498999999999999,3.00099698131059E-17));
#4945=CARTESIAN_POINT('Origin',(0.,-0.0498999999999999,0.));
#4946=CARTESIAN_POINT('',(-0.26,-0.02,-3.18408167778312E-17));
#4947=CARTESIAN_POINT('Origin',(0.,-0.995,0.));
#4948=CARTESIAN_POINT('',(-0.24505,-0.995,-3.00099698131059E-17));
#4949=CARTESIAN_POINT('Origin',(0.115470053837925,-0.5,-0.2));
#4950=CARTESIAN_POINT('',(0.23094010767585,-0.5,0.));
#4951=CARTESIAN_POINT('',(0.115470053837925,-0.5,-0.2));
#4952=CARTESIAN_POINT('',(0.23094010767585,-0.5,0.));
#4953=CARTESIAN_POINT('',(0.115470053837925,-0.8,-0.2));
#4954=CARTESIAN_POINT('',(0.115470053837925,-0.5,-0.2));
#4955=CARTESIAN_POINT('',(0.23094010767585,-0.8,0.));
#4956=CARTESIAN_POINT('',(0.23094010767585,-0.8,0.));
#4957=CARTESIAN_POINT('',(0.23094010767585,-0.5,0.));
#4958=CARTESIAN_POINT('Origin',(-0.115470053837925,-0.5,-0.2));
#4959=CARTESIAN_POINT('',(-0.115470053837925,-0.5,-0.2));
#4960=CARTESIAN_POINT('',(0.115470053837925,-0.5,-0.2));
#4961=CARTESIAN_POINT('',(-0.115470053837925,-0.8,-0.2));
#4962=CARTESIAN_POINT('',(-0.115470053837925,-0.5,-0.2));
#4963=CARTESIAN_POINT('',(0.115470053837925,-0.8,-0.2));
#4964=CARTESIAN_POINT('Origin',(-0.23094010767585,-0.5,-2.77555756156289E-17));
#4965=CARTESIAN_POINT('',(-0.23094010767585,-0.5,-2.82820063659975E-17));
#4966=CARTESIAN_POINT('',(-0.115470053837925,-0.5,-0.2));
#4967=CARTESIAN_POINT('',(-0.23094010767585,-0.8,-2.77555756156289E-17));
#4968=CARTESIAN_POINT('',(-0.23094010767585,-0.5,-2.82820063659975E-17));
#4969=CARTESIAN_POINT('',(-0.115470053837925,-0.8,-0.2));
#4970=CARTESIAN_POINT('Origin',(-0.115470053837925,-0.5,0.2));
#4971=CARTESIAN_POINT('',(-0.115470053837925,-0.5,0.2));
#4972=CARTESIAN_POINT('',(-0.23094010767585,-0.5,-2.82820063659975E-17));
#4973=CARTESIAN_POINT('',(-0.115470053837925,-0.8,0.2));
#4974=CARTESIAN_POINT('',(-0.115470053837925,-0.5,0.2));
#4975=CARTESIAN_POINT('',(-0.23094010767585,-0.8,-2.82820063659975E-17));
#4976=CARTESIAN_POINT('Origin',(0.115470053837925,-0.5,0.2));
#4977=CARTESIAN_POINT('',(0.115470053837925,-0.5,0.2));
#4978=CARTESIAN_POINT('',(-0.115470053837925,-0.5,0.2));
#4979=CARTESIAN_POINT('',(0.115470053837925,-0.8,0.2));
#4980=CARTESIAN_POINT('',(0.115470053837925,-0.5,0.2));
#4981=CARTESIAN_POINT('',(-0.115470053837925,-0.8,0.2));
#4982=CARTESIAN_POINT('Origin',(0.23094010767585,-0.5,0.));
#4983=CARTESIAN_POINT('',(0.115470053837925,-0.5,0.2));
#4984=CARTESIAN_POINT('',(0.115470053837925,-0.8,0.2));
#4985=CARTESIAN_POINT('Origin',(0.,-0.5,0.));
#4986=CARTESIAN_POINT('Origin',(0.,-0.8,0.));
#4987=CARTESIAN_POINT('',(0.,0.,0.));
#4988=CARTESIAN_POINT('Origin',(-0.1,0.82,-0.3));
#4989=CARTESIAN_POINT('',(0.,0.82,-0.3));
#4990=CARTESIAN_POINT('',(0.,1.,-0.3));
#4991=CARTESIAN_POINT('',(0.,0.41,-0.3));
#4992=CARTESIAN_POINT('',(10.,0.82,-0.3));
#4993=CARTESIAN_POINT('',(-0.1,0.82,-0.3));
#4994=CARTESIAN_POINT('',(10.,1.,-0.3));
#4995=CARTESIAN_POINT('',(10.,0.41,-0.3));
#4996=CARTESIAN_POINT('',(-0.05,1.,-0.3));
#4997=CARTESIAN_POINT('Origin',(-0.1,0.82,-0.55));
#4998=CARTESIAN_POINT('',(0.,0.82,-0.55));
#4999=CARTESIAN_POINT('',(0.,0.82,-0.275));
#5000=CARTESIAN_POINT('',(10.,0.82,-0.55));
#5001=CARTESIAN_POINT('',(-0.1,0.82,-0.55));
#5002=CARTESIAN_POINT('',(10.,0.82,-0.275));
#5003=CARTESIAN_POINT('Origin',(-0.1,0.67,-0.55));
#5004=CARTESIAN_POINT('',(0.,0.67,-0.55));
#5005=CARTESIAN_POINT('',(0.,0.335,-0.55));
#5006=CARTESIAN_POINT('',(10.,0.67,-0.55));
#5007=CARTESIAN_POINT('',(-0.1,0.67,-0.55));
#5008=CARTESIAN_POINT('',(10.,0.335,-0.55));
#5009=CARTESIAN_POINT('Origin',(-0.1,0.42,-0.3));
#5010=CARTESIAN_POINT('',(0.,0.42,-0.3));
#5011=CARTESIAN_POINT('',(0.,0.24,-0.12));
#5012=CARTESIAN_POINT('',(10.,0.42,-0.3));
#5013=CARTESIAN_POINT('',(-0.1,0.42,-0.3));
#5014=CARTESIAN_POINT('',(10.,0.24,-0.12));
#5015=CARTESIAN_POINT('Origin',(-0.1,0.42,0.3));
#5016=CARTESIAN_POINT('',(0.,0.42,0.3));
#5017=CARTESIAN_POINT('',(0.,0.42,0.15));
#5018=CARTESIAN_POINT('',(10.,0.42,0.3));
#5019=CARTESIAN_POINT('',(-0.1,0.42,0.3));
#5020=CARTESIAN_POINT('',(10.,0.42,0.15));
#5021=CARTESIAN_POINT('Origin',(-0.1,0.67,0.55));
#5022=CARTESIAN_POINT('',(0.,0.67,0.55));
#5023=CARTESIAN_POINT('',(6.93889390390723E-18,0.365,0.245));
#5024=CARTESIAN_POINT('',(10.,0.67,0.55));
#5025=CARTESIAN_POINT('',(-0.1,0.67,0.55));
#5026=CARTESIAN_POINT('',(10.,0.365,0.245));
#5027=CARTESIAN_POINT('Origin',(-0.1,0.82,0.55));
#5028=CARTESIAN_POINT('',(0.,0.82,0.55));
#5029=CARTESIAN_POINT('',(0.,0.41,0.55));
#5030=CARTESIAN_POINT('',(10.,0.82,0.55));
#5031=CARTESIAN_POINT('',(-0.1,0.82,0.55));
#5032=CARTESIAN_POINT('',(10.,0.41,0.55));
#5033=CARTESIAN_POINT('Origin',(-0.1,0.82,0.3));
#5034=CARTESIAN_POINT('',(0.,0.82,0.3));
#5035=CARTESIAN_POINT('',(0.,0.82,0.15));
#5036=CARTESIAN_POINT('',(10.,0.82,0.3));
#5037=CARTESIAN_POINT('',(-0.1,0.82,0.3));
#5038=CARTESIAN_POINT('',(10.,0.82,0.15));
#5039=CARTESIAN_POINT('Origin',(-0.1,1.05,0.3));
#5040=CARTESIAN_POINT('',(0.,1.,0.3));
#5041=CARTESIAN_POINT('',(0.,0.525,0.3));
#5042=CARTESIAN_POINT('',(10.,1.,0.3));
#5043=CARTESIAN_POINT('',(-0.05,1.,0.3));
#5044=CARTESIAN_POINT('',(10.,0.525,0.3));
#5045=CARTESIAN_POINT('Origin',(-0.1,-0.3,-0.82));
#5046=CARTESIAN_POINT('',(0.,-0.3,-0.82));
#5047=CARTESIAN_POINT('',(0.,-0.3,-1.));
#5048=CARTESIAN_POINT('',(0.,-0.3,-0.41));
#5049=CARTESIAN_POINT('',(10.,-0.3,-0.82));
#5050=CARTESIAN_POINT('',(-0.1,-0.3,-0.82));
#5051=CARTESIAN_POINT('',(10.,-0.3,-1.));
#5052=CARTESIAN_POINT('',(10.,-0.3,-0.41));
#5053=CARTESIAN_POINT('',(-0.05,-0.3,-1.));
#5054=CARTESIAN_POINT('Origin',(-0.1,-0.55,-0.82));
#5055=CARTESIAN_POINT('',(0.,-0.55,-0.82));
#5056=CARTESIAN_POINT('',(0.,-0.275,-0.82));
#5057=CARTESIAN_POINT('',(10.,-0.55,-0.82));
#5058=CARTESIAN_POINT('',(-0.1,-0.55,-0.82));
#5059=CARTESIAN_POINT('',(10.,-0.275,-0.82));
#5060=CARTESIAN_POINT('Origin',(-0.1,-0.55,-0.67));
#5061=CARTESIAN_POINT('',(0.,-0.55,-0.67));
#5062=CARTESIAN_POINT('',(0.,-0.55,-0.335));
#5063=CARTESIAN_POINT('',(10.,-0.55,-0.67));
#5064=CARTESIAN_POINT('',(-0.1,-0.55,-0.67));
#5065=CARTESIAN_POINT('',(10.,-0.55,-0.335));
#5066=CARTESIAN_POINT('Origin',(-0.1,-0.3,-0.42));
#5067=CARTESIAN_POINT('',(0.,-0.3,-0.42));
#5068=CARTESIAN_POINT('',(0.,-0.12,-0.24));
#5069=CARTESIAN_POINT('',(10.,-0.3,-0.42));
#5070=CARTESIAN_POINT('',(-0.1,-0.3,-0.42));
#5071=CARTESIAN_POINT('',(10.,-0.12,-0.24));
#5072=CARTESIAN_POINT('Origin',(-0.1,0.3,-0.42));
#5073=CARTESIAN_POINT('',(0.,0.3,-0.42));
#5074=CARTESIAN_POINT('',(0.,0.15,-0.42));
#5075=CARTESIAN_POINT('',(10.,0.3,-0.42));
#5076=CARTESIAN_POINT('',(-0.1,0.3,-0.42));
#5077=CARTESIAN_POINT('',(10.,0.15,-0.42));
#5078=CARTESIAN_POINT('Origin',(-0.1,0.55,-0.67));
#5079=CARTESIAN_POINT('',(0.,0.55,-0.67));
#5080=CARTESIAN_POINT('',(0.,0.245,-0.365));
#5081=CARTESIAN_POINT('',(10.,0.55,-0.67));
#5082=CARTESIAN_POINT('',(-0.1,0.55,-0.67));
#5083=CARTESIAN_POINT('',(10.,0.245,-0.365));
#5084=CARTESIAN_POINT('Origin',(-0.1,0.55,-0.82));
#5085=CARTESIAN_POINT('',(0.,0.55,-0.82));
#5086=CARTESIAN_POINT('',(0.,0.55,-0.41));
#5087=CARTESIAN_POINT('',(10.,0.55,-0.82));
#5088=CARTESIAN_POINT('',(-0.1,0.55,-0.82));
#5089=CARTESIAN_POINT('',(10.,0.55,-0.41));
#5090=CARTESIAN_POINT('Origin',(-0.1,0.3,-0.82));
#5091=CARTESIAN_POINT('',(0.,0.3,-0.82));
#5092=CARTESIAN_POINT('',(0.,0.15,-0.82));
#5093=CARTESIAN_POINT('',(10.,0.3,-0.82));
#5094=CARTESIAN_POINT('',(-0.1,0.3,-0.82));
#5095=CARTESIAN_POINT('',(10.,0.15,-0.82));
#5096=CARTESIAN_POINT('Origin',(-0.1,0.3,-1.05));
#5097=CARTESIAN_POINT('',(0.,0.3,-1.));
#5098=CARTESIAN_POINT('',(0.,0.3,-0.525));
#5099=CARTESIAN_POINT('',(10.,0.3,-1.));
#5100=CARTESIAN_POINT('',(-0.05,0.3,-1.));
#5101=CARTESIAN_POINT('',(10.,0.3,-0.525));
#5102=CARTESIAN_POINT('Origin',(-0.1,-0.82,0.3));
#5103=CARTESIAN_POINT('',(0.,-0.82,0.3));
#5104=CARTESIAN_POINT('',(0.,-1.,0.3));
#5105=CARTESIAN_POINT('',(0.,-0.41,0.3));
#5106=CARTESIAN_POINT('',(10.,-0.82,0.3));
#5107=CARTESIAN_POINT('',(-0.1,-0.82,0.3));
#5108=CARTESIAN_POINT('',(10.,-1.,0.3));
#5109=CARTESIAN_POINT('',(10.,-0.41,0.3));
#5110=CARTESIAN_POINT('',(-0.05,-1.,0.3));
#5111=CARTESIAN_POINT('Origin',(-0.1,-0.82,0.55));
#5112=CARTESIAN_POINT('',(0.,-0.82,0.55));
#5113=CARTESIAN_POINT('',(0.,-0.82,0.275));
#5114=CARTESIAN_POINT('',(10.,-0.82,0.55));
#5115=CARTESIAN_POINT('',(-0.1,-0.82,0.55));
#5116=CARTESIAN_POINT('',(10.,-0.82,0.275));
#5117=CARTESIAN_POINT('Origin',(-0.1,-0.67,0.55));
#5118=CARTESIAN_POINT('',(0.,-0.67,0.55));
#5119=CARTESIAN_POINT('',(0.,-0.335,0.55));
#5120=CARTESIAN_POINT('',(10.,-0.67,0.55));
#5121=CARTESIAN_POINT('',(-0.1,-0.67,0.55));
#5122=CARTESIAN_POINT('',(10.,-0.335,0.55));
#5123=CARTESIAN_POINT('Origin',(-0.1,-0.42,0.3));
#5124=CARTESIAN_POINT('',(0.,-0.42,0.3));
#5125=CARTESIAN_POINT('',(-6.93889390390723E-18,-0.24,0.12));
#5126=CARTESIAN_POINT('',(10.,-0.42,0.3));
#5127=CARTESIAN_POINT('',(-0.1,-0.42,0.3));
#5128=CARTESIAN_POINT('',(10.,-0.24,0.12));
#5129=CARTESIAN_POINT('Origin',(-0.1,-0.42,-0.3));
#5130=CARTESIAN_POINT('',(0.,-0.42,-0.3));
#5131=CARTESIAN_POINT('',(0.,-0.42,-0.15));
#5132=CARTESIAN_POINT('',(10.,-0.42,-0.3));
#5133=CARTESIAN_POINT('',(-0.1,-0.42,-0.3));
#5134=CARTESIAN_POINT('',(10.,-0.42,-0.15));
#5135=CARTESIAN_POINT('Origin',(-0.1,-0.67,-0.55));
#5136=CARTESIAN_POINT('',(0.,-0.67,-0.55));
#5137=CARTESIAN_POINT('',(0.,-0.365,-0.245));
#5138=CARTESIAN_POINT('',(10.,-0.67,-0.55));
#5139=CARTESIAN_POINT('',(-0.1,-0.67,-0.55));
#5140=CARTESIAN_POINT('',(10.,-0.365,-0.245));
#5141=CARTESIAN_POINT('Origin',(-0.1,-0.82,-0.55));
#5142=CARTESIAN_POINT('',(0.,-0.82,-0.55));
#5143=CARTESIAN_POINT('',(0.,-0.41,-0.55));
#5144=CARTESIAN_POINT('',(10.,-0.82,-0.55));
#5145=CARTESIAN_POINT('',(-0.1,-0.82,-0.55));
#5146=CARTESIAN_POINT('',(10.,-0.41,-0.55));
#5147=CARTESIAN_POINT('Origin',(-0.1,-0.82,-0.3));
#5148=CARTESIAN_POINT('',(0.,-0.82,-0.3));
#5149=CARTESIAN_POINT('',(0.,-0.82,-0.15));
#5150=CARTESIAN_POINT('',(10.,-0.82,-0.3));
#5151=CARTESIAN_POINT('',(-0.1,-0.82,-0.3));
#5152=CARTESIAN_POINT('',(10.,-0.82,-0.15));
#5153=CARTESIAN_POINT('Origin',(-0.1,-1.05,-0.3));
#5154=CARTESIAN_POINT('',(0.,-1.,-0.3));
#5155=CARTESIAN_POINT('',(0.,-0.525,-0.3));
#5156=CARTESIAN_POINT('',(10.,-1.,-0.3));
#5157=CARTESIAN_POINT('',(-0.05,-1.,-0.3));
#5158=CARTESIAN_POINT('',(10.,-0.525,-0.3));
#5159=CARTESIAN_POINT('Origin',(-0.1,0.3,0.82));
#5160=CARTESIAN_POINT('',(0.,0.3,0.82));
#5161=CARTESIAN_POINT('',(0.,0.3,1.));
#5162=CARTESIAN_POINT('',(0.,0.3,0.41));
#5163=CARTESIAN_POINT('',(10.,0.3,0.82));
#5164=CARTESIAN_POINT('',(-0.1,0.3,0.82));
#5165=CARTESIAN_POINT('',(10.,0.3,1.));
#5166=CARTESIAN_POINT('',(10.,0.3,0.41));
#5167=CARTESIAN_POINT('',(-0.05,0.3,1.));
#5168=CARTESIAN_POINT('Origin',(-0.1,0.55,0.82));
#5169=CARTESIAN_POINT('',(0.,0.55,0.82));
#5170=CARTESIAN_POINT('',(0.,0.275,0.82));
#5171=CARTESIAN_POINT('',(10.,0.55,0.82));
#5172=CARTESIAN_POINT('',(-0.1,0.55,0.82));
#5173=CARTESIAN_POINT('',(10.,0.275,0.82));
#5174=CARTESIAN_POINT('Origin',(-0.1,0.55,0.67));
#5175=CARTESIAN_POINT('',(0.,0.55,0.67));
#5176=CARTESIAN_POINT('',(0.,0.55,0.335));
#5177=CARTESIAN_POINT('',(10.,0.55,0.67));
#5178=CARTESIAN_POINT('',(-0.1,0.55,0.67));
#5179=CARTESIAN_POINT('',(10.,0.55,0.335));
#5180=CARTESIAN_POINT('Origin',(-0.1,0.3,0.42));
#5181=CARTESIAN_POINT('',(0.,0.3,0.42));
#5182=CARTESIAN_POINT('',(6.93889390390723E-18,0.12,0.24));
#5183=CARTESIAN_POINT('',(10.,0.3,0.42));
#5184=CARTESIAN_POINT('',(-0.1,0.3,0.42));
#5185=CARTESIAN_POINT('',(10.,0.12,0.24));
#5186=CARTESIAN_POINT('Origin',(-0.1,-0.3,0.42));
#5187=CARTESIAN_POINT('',(0.,-0.3,0.42));
#5188=CARTESIAN_POINT('',(0.,-0.15,0.42));
#5189=CARTESIAN_POINT('',(10.,-0.3,0.42));
#5190=CARTESIAN_POINT('',(-0.1,-0.3,0.42));
#5191=CARTESIAN_POINT('',(10.,-0.15,0.42));
#5192=CARTESIAN_POINT('Origin',(-0.1,-0.55,0.67));
#5193=CARTESIAN_POINT('',(0.,-0.55,0.67));
#5194=CARTESIAN_POINT('',(6.93889390390723E-18,-0.245,0.365));
#5195=CARTESIAN_POINT('',(10.,-0.55,0.67));
#5196=CARTESIAN_POINT('',(-0.1,-0.55,0.67));
#5197=CARTESIAN_POINT('',(10.,-0.245,0.365));
#5198=CARTESIAN_POINT('Origin',(-0.1,-0.55,0.82));
#5199=CARTESIAN_POINT('',(0.,-0.55,0.82));
#5200=CARTESIAN_POINT('',(0.,-0.55,0.41));
#5201=CARTESIAN_POINT('',(10.,-0.55,0.82));
#5202=CARTESIAN_POINT('',(-0.1,-0.55,0.82));
#5203=CARTESIAN_POINT('',(10.,-0.55,0.41));
#5204=CARTESIAN_POINT('Origin',(-0.1,-0.3,0.82));
#5205=CARTESIAN_POINT('',(0.,-0.3,0.82));
#5206=CARTESIAN_POINT('',(0.,-0.15,0.82));
#5207=CARTESIAN_POINT('',(10.,-0.3,0.82));
#5208=CARTESIAN_POINT('',(-0.1,-0.3,0.82));
#5209=CARTESIAN_POINT('',(10.,-0.15,0.82));
#5210=CARTESIAN_POINT('Origin',(-0.1,-0.3,1.05));
#5211=CARTESIAN_POINT('',(0.,-0.3,1.));
#5212=CARTESIAN_POINT('',(0.,-0.3,0.525));
#5213=CARTESIAN_POINT('',(10.,-0.3,1.));
#5214=CARTESIAN_POINT('',(-0.05,-0.3,1.));
#5215=CARTESIAN_POINT('',(10.,-0.3,0.525));
#5216=CARTESIAN_POINT('Origin',(-0.1,0.,0.));
#5217=CARTESIAN_POINT('',(0.,-2.57175827820944E-17,0.21));
#5218=CARTESIAN_POINT('Origin',(0.,0.,0.));
#5219=CARTESIAN_POINT('',(10.,2.57175827820944E-17,0.21));
#5220=CARTESIAN_POINT('',(-0.1,-2.57175827820944E-17,0.21));
#5221=CARTESIAN_POINT('Origin',(10.,0.,0.));
#5222=CARTESIAN_POINT('Origin',(0.,1.,-1.));
#5223=CARTESIAN_POINT('',(0.,1.,1.));
#5224=CARTESIAN_POINT('',(0.,1.,-1.));
#5225=CARTESIAN_POINT('',(10.,1.,1.));
#5226=CARTESIAN_POINT('',(0.,1.,1.));
#5227=CARTESIAN_POINT('',(10.,1.,-1.));
#5228=CARTESIAN_POINT('Origin',(0.,1.,-1.));
#5229=CARTESIAN_POINT('',(10.,1.,-1.));
#5230=CARTESIAN_POINT('',(10.,1.,-1.));
#5231=CARTESIAN_POINT('',(0.,1.,-1.));
#5232=CARTESIAN_POINT('',(0.,1.,-1.));
#5233=CARTESIAN_POINT('',(0.,1.,-1.));
#5234=CARTESIAN_POINT('Origin',(0.,-1.,-1.));
#5235=CARTESIAN_POINT('',(0.,-1.,-1.));
#5236=CARTESIAN_POINT('',(10.,-1.,-1.));
#5237=CARTESIAN_POINT('Origin',(0.,-1.,-1.));
#5238=CARTESIAN_POINT('',(10.,-1.,-1.));
#5239=CARTESIAN_POINT('',(10.,-1.,-1.));
#5240=CARTESIAN_POINT('',(0.,-1.,-1.));
#5241=CARTESIAN_POINT('',(0.,-1.,-1.));
#5242=CARTESIAN_POINT('',(0.,-1.,-1.));
#5243=CARTESIAN_POINT('Origin',(0.,-1.,1.));
#5244=CARTESIAN_POINT('',(0.,-1.,1.));
#5245=CARTESIAN_POINT('',(10.,-1.,1.));
#5246=CARTESIAN_POINT('Origin',(0.,-1.,1.));
#5247=CARTESIAN_POINT('',(10.,-1.,1.));
#5248=CARTESIAN_POINT('',(10.,-1.,1.));
#5249=CARTESIAN_POINT('',(0.,-1.,1.));
#5250=CARTESIAN_POINT('',(0.,-1.,1.));
#5251=CARTESIAN_POINT('',(0.,-1.,1.));
#5252=CARTESIAN_POINT('Origin',(0.,1.,1.));
#5253=CARTESIAN_POINT('',(0.,1.,1.));
#5254=CARTESIAN_POINT('',(10.,1.,1.));
#5255=CARTESIAN_POINT('Origin',(0.,1.,1.));
#5256=CARTESIAN_POINT('',(10.,1.,1.));
#5257=CARTESIAN_POINT('',(0.,1.,1.));
#5258=CARTESIAN_POINT('Origin',(10.,0.,0.));
#5259=CARTESIAN_POINT('Origin',(0.,0.,0.));
#5260=CARTESIAN_POINT('',(0.,0.,0.));
#5261=CARTESIAN_POINT('Origin',(0.,-1.935,0.));
#5262=CARTESIAN_POINT('',(-0.3933,-3.9267,4.81653586104654E-17));
#5263=CARTESIAN_POINT('Origin',(0.,-3.9267,0.));
#5264=CARTESIAN_POINT('',(-0.3933,0.,-4.81653586104654E-17));
#5265=CARTESIAN_POINT('',(-0.3933,-1.935,-4.81653586104654E-17));
#5266=CARTESIAN_POINT('Origin',(0.,0.,0.));
#5267=CARTESIAN_POINT('Origin',(0.,-3.96,0.));
#5268=CARTESIAN_POINT('',(-0.32,-4.,-3.91886975727153E-17));
#5269=CARTESIAN_POINT('Origin',(0.,-4.,0.));
#5270=CARTESIAN_POINT('',(-0.36,-3.96,-4.40872847693047E-17));
#5271=CARTESIAN_POINT('Origin',(0.,-4.,0.));
#5272=CARTESIAN_POINT('Origin',(0.,0.462722715486149,0.));
#5273=CARTESIAN_POINT('',(-0.6175,0.53,-7.5621939847349E-17));
#5274=CARTESIAN_POINT('Origin',(0.,0.53,0.));
#5275=CARTESIAN_POINT('',(-0.750555349946514,0.453180457891261,-9.19165206894919E-17));
#5276=CARTESIAN_POINT('',(-0.734027674973257,0.462722715486149,-8.98924642641573E-17));
#5277=CARTESIAN_POINT('',(-0.375277674973257,0.453180457891261,0.65));
#5278=CARTESIAN_POINT('Ctrl Pts',(-0.375277674973257,0.45318045789126,0.65));
#5279=CARTESIAN_POINT('Ctrl Pts',(-0.562916512459968,0.561513791224244,
0.324999999999856));
#5280=CARTESIAN_POINT('Ctrl Pts',(-0.750555349946514,0.45318045789126,-9.19165206894919E-17));
#5281=CARTESIAN_POINT('',(0.375277674973257,0.453180457891261,0.65));
#5282=CARTESIAN_POINT('Ctrl Pts',(0.375277674973257,0.453180457891261,0.65));
#5283=CARTESIAN_POINT('Ctrl Pts',(-1.66922031752392E-13,0.561513791224244,
0.65));
#5284=CARTESIAN_POINT('Ctrl Pts',(-0.375277674973257,0.45318045789126,0.65));
#5285=CARTESIAN_POINT('',(0.750555349946514,0.453180457891261,0.));
#5286=CARTESIAN_POINT('Ctrl Pts',(0.750555349946514,0.453180457891261,0.));
#5287=CARTESIAN_POINT('Ctrl Pts',(0.562916512459802,0.561513791224244,0.325000000000144));
#5288=CARTESIAN_POINT('Ctrl Pts',(0.375277674973257,0.45318045789126,0.65));
#5289=CARTESIAN_POINT('',(0.375277674973257,0.453180457891261,-0.65));
#5290=CARTESIAN_POINT('Ctrl Pts',(0.375277674973257,0.45318045789126,-0.65));
#5291=CARTESIAN_POINT('Ctrl Pts',(0.562916512459968,0.561513791224244,-0.324999999999855));
#5292=CARTESIAN_POINT('Ctrl Pts',(0.750555349946514,0.453180457891261,0.));
#5293=CARTESIAN_POINT('',(-0.375277674973257,0.45318045789126,-0.65));
#5294=CARTESIAN_POINT('Ctrl Pts',(-0.375277674973257,0.453180457891261,
-0.65));
#5295=CARTESIAN_POINT('Ctrl Pts',(1.66866520601161E-13,0.561513791224244,
-0.65));
#5296=CARTESIAN_POINT('Ctrl Pts',(0.375277674973257,0.45318045789126,-0.65));
#5297=CARTESIAN_POINT('Ctrl Pts',(-0.750555349946514,0.453180457891261,
-9.19165206894919E-17));
#5298=CARTESIAN_POINT('Ctrl Pts',(-0.562916512459802,0.561513791224244,
-0.325000000000144));
#5299=CARTESIAN_POINT('Ctrl Pts',(-0.375277674973257,0.45318045789126,-0.65));
#5300=CARTESIAN_POINT('Origin',(0.375277674973257,0.,-0.65));
#5301=CARTESIAN_POINT('',(0.375277674973257,0.,-0.65));
#5302=CARTESIAN_POINT('',(0.375277674973257,0.,-0.65));
#5303=CARTESIAN_POINT('',(-0.375277674973257,0.,-0.65));
#5304=CARTESIAN_POINT('',(0.375277674973257,0.,-0.65));
#5305=CARTESIAN_POINT('',(-0.375277674973257,0.,-0.65));
#5306=CARTESIAN_POINT('Origin',(0.750555349946514,0.,0.));
#5307=CARTESIAN_POINT('',(0.750555349946514,0.,0.));
#5308=CARTESIAN_POINT('',(0.750555349946514,0.,0.));
#5309=CARTESIAN_POINT('',(0.750555349946514,0.,0.));
#5310=CARTESIAN_POINT('Origin',(0.375277674973257,0.,0.65));
#5311=CARTESIAN_POINT('',(0.375277674973257,0.,0.65));
#5312=CARTESIAN_POINT('',(0.375277674973257,0.,0.65));
#5313=CARTESIAN_POINT('',(0.375277674973257,0.,0.65));
#5314=CARTESIAN_POINT('Origin',(-0.375277674973257,0.,0.65));
#5315=CARTESIAN_POINT('',(-0.375277674973257,0.,0.65));
#5316=CARTESIAN_POINT('',(-0.375277674973257,0.,0.65));
#5317=CARTESIAN_POINT('',(-0.375277674973257,0.,0.65));
#5318=CARTESIAN_POINT('Origin',(-0.750555349946514,0.,-9.19165206894919E-17));
#5319=CARTESIAN_POINT('',(-0.750555349946514,0.,-9.19165206894919E-17));
#5320=CARTESIAN_POINT('',(-0.750555349946514,0.,-9.19165206894919E-17));
#5321=CARTESIAN_POINT('',(-0.750555349946514,0.,-9.19165206894919E-17));
#5322=CARTESIAN_POINT('Origin',(-0.375277674973257,0.,-0.65));
#5323=CARTESIAN_POINT('',(-0.375277674973257,0.,-0.65));
#5324=CARTESIAN_POINT('Origin',(0.,0.53,-1.11022302462516E-16));
#5325=CARTESIAN_POINT('Origin',(0.,0.,-1.11022302462516E-16));
#5326=CARTESIAN_POINT('',(0.,0.,0.));
#5327=CARTESIAN_POINT('',(0.,0.,0.));
#5328=CARTESIAN_POINT('Origin',(14.,-0.6,4.7));
#5329=CARTESIAN_POINT('',(13.835,-0.6,4.8));
#5330=CARTESIAN_POINT('Origin',(14.,-0.6,4.8));
#5331=CARTESIAN_POINT('',(13.835,-0.6,5.6));
#5332=CARTESIAN_POINT('',(13.835,-0.6,4.7));
#5333=CARTESIAN_POINT('Origin',(14.,-0.6,5.6));
#5334=CARTESIAN_POINT('Origin',(14.,0.6,4.7));
#5335=CARTESIAN_POINT('',(13.835,0.6,4.8));
#5336=CARTESIAN_POINT('Origin',(14.,0.6,4.8));
#5337=CARTESIAN_POINT('',(13.835,0.6,5.6));
#5338=CARTESIAN_POINT('',(13.835,0.6,4.7));
#5339=CARTESIAN_POINT('Origin',(14.,0.6,5.6));
#5340=CARTESIAN_POINT('Origin',(5.,0.,5.6));
#5341=CARTESIAN_POINT('',(6.49666295470958,1.,5.6));
#5342=CARTESIAN_POINT('',(3.2,-2.20436423846524E-16,5.6));
#5343=CARTESIAN_POINT('Origin',(5.,0.,5.6));
#5344=CARTESIAN_POINT('',(6.49666295470958,-1.,5.6));
#5345=CARTESIAN_POINT('Origin',(5.,0.,5.6));
#5346=CARTESIAN_POINT('',(15.,-1.,5.6));
#5347=CARTESIAN_POINT('',(5.,-1.,5.6));
#5348=CARTESIAN_POINT('',(15.,1.,5.6));
#5349=CARTESIAN_POINT('',(15.,-1.,5.6));
#5350=CARTESIAN_POINT('',(15.,1.,5.6));
#5351=CARTESIAN_POINT('',(4.575,-5.20474889637625E-17,5.6));
#5352=CARTESIAN_POINT('Origin',(5.,0.,5.6));
#5353=CARTESIAN_POINT('Origin',(15.,1.,4.8));
#5354=CARTESIAN_POINT('',(6.49666295470958,1.,4.8));
#5355=CARTESIAN_POINT('',(6.49666295470958,1.,4.4));
#5356=CARTESIAN_POINT('',(15.,1.,4.8));
#5357=CARTESIAN_POINT('',(15.,1.,4.8));
#5358=CARTESIAN_POINT('',(15.,1.,4.8));
#5359=CARTESIAN_POINT('Origin',(15.,-1.,4.8));
#5360=CARTESIAN_POINT('',(15.,-1.,4.8));
#5361=CARTESIAN_POINT('',(15.,-1.,4.8));
#5362=CARTESIAN_POINT('',(15.,-1.,4.8));
#5363=CARTESIAN_POINT('Origin',(5.,-1.,4.8));
#5364=CARTESIAN_POINT('',(6.49666295470958,-1.,4.8));
#5365=CARTESIAN_POINT('',(6.49666295470958,-1.,4.4));
#5366=CARTESIAN_POINT('',(5.,-1.,4.8));
#5367=CARTESIAN_POINT('Origin',(10.,0.,4.8));
#5368=CARTESIAN_POINT('Origin',(5.,0.,4.8));
#5369=CARTESIAN_POINT('Origin',(5.,0.,4.4));
#5370=CARTESIAN_POINT('',(3.2,-2.20436423846524E-16,4.4));
#5371=CARTESIAN_POINT('',(3.2,-2.20436423846524E-16,4.4));
#5372=CARTESIAN_POINT('Origin',(5.,0.,4.4));
#5373=CARTESIAN_POINT('Origin',(5.,0.,4.4));
#5374=CARTESIAN_POINT('',(4.575,-5.20474889637625E-17,4.4));
#5375=CARTESIAN_POINT('',(4.575,-5.20474889637625E-17,4.4));
#5376=CARTESIAN_POINT('Origin',(5.,0.,4.4));
#5377=CARTESIAN_POINT('Origin',(5.,0.,4.4));
#5378=CARTESIAN_POINT('',(0.,0.,0.));
#5379=CARTESIAN_POINT('Origin',(14.,-0.6,6.4));
#5380=CARTESIAN_POINT('',(13.6,-0.6,6.4));
#5381=CARTESIAN_POINT('Origin',(14.,-0.6,6.4));
#5382=CARTESIAN_POINT('',(13.6,-0.6,8.6));
#5383=CARTESIAN_POINT('',(13.6,-0.6,6.4));
#5384=CARTESIAN_POINT('Origin',(14.,-0.6,8.6));
#5385=CARTESIAN_POINT('Origin',(14.,-0.6,6.4));
#5386=CARTESIAN_POINT('',(13.775,-0.6,6.4));
#5387=CARTESIAN_POINT('Origin',(14.,-0.6,6.4));
#5388=CARTESIAN_POINT('Origin',(14.,0.6,6.4));
#5389=CARTESIAN_POINT('',(13.6,0.6,6.4));
#5390=CARTESIAN_POINT('Origin',(14.,0.6,6.4));
#5391=CARTESIAN_POINT('',(13.6,0.6,8.6));
#5392=CARTESIAN_POINT('',(13.6,0.6,6.4));
#5393=CARTESIAN_POINT('Origin',(14.,0.6,8.6));
#5394=CARTESIAN_POINT('Origin',(14.,0.6,6.4));
#5395=CARTESIAN_POINT('',(13.775,0.6,6.4));
#5396=CARTESIAN_POINT('Origin',(14.,0.6,6.4));
#5397=CARTESIAN_POINT('Origin',(14.,-0.6,5.5));
#5398=CARTESIAN_POINT('',(13.775,-0.6,5.6));
#5399=CARTESIAN_POINT('Origin',(14.,-0.6,5.6));
#5400=CARTESIAN_POINT('',(13.775,-0.6,5.5));
#5401=CARTESIAN_POINT('Origin',(14.,0.6,5.5));
#5402=CARTESIAN_POINT('',(13.775,0.6,5.6));
#5403=CARTESIAN_POINT('Origin',(14.,0.6,5.6));
#5404=CARTESIAN_POINT('',(13.775,0.6,5.5));
#5405=CARTESIAN_POINT('Origin',(15.,2.5,5.6));
#5406=CARTESIAN_POINT('',(15.,2.5,5.6));
#5407=CARTESIAN_POINT('',(13.,2.5,5.6));
#5408=CARTESIAN_POINT('',(15.,2.5,5.6));
#5409=CARTESIAN_POINT('',(13.,2.5,8.6));
#5410=CARTESIAN_POINT('',(13.,2.5,5.6));
#5411=CARTESIAN_POINT('',(15.,2.5,8.6));
#5412=CARTESIAN_POINT('',(15.,2.5,8.6));
#5413=CARTESIAN_POINT('',(15.,2.5,5.6));
#5414=CARTESIAN_POINT('Origin',(15.,-2.5,5.6));
#5415=CARTESIAN_POINT('',(15.,-2.5,5.6));
#5416=CARTESIAN_POINT('',(15.,-2.5,5.6));
#5417=CARTESIAN_POINT('',(15.,-2.5,8.6));
#5418=CARTESIAN_POINT('',(15.,-2.5,8.6));
#5419=CARTESIAN_POINT('',(15.,-2.5,5.6));
#5420=CARTESIAN_POINT('Origin',(13.,-2.5,5.6));
#5421=CARTESIAN_POINT('',(13.,-2.5,5.6));
#5422=CARTESIAN_POINT('',(13.,-2.5,5.6));
#5423=CARTESIAN_POINT('',(13.,-2.5,8.6));
#5424=CARTESIAN_POINT('',(13.,-2.5,8.6));
#5425=CARTESIAN_POINT('',(13.,-2.5,5.6));
#5426=CARTESIAN_POINT('Origin',(13.,2.5,5.6));
#5427=CARTESIAN_POINT('',(13.,2.5,5.6));
#5428=CARTESIAN_POINT('',(13.,2.5,8.6));
#5429=CARTESIAN_POINT('Origin',(14.,0.,8.6));
#5430=CARTESIAN_POINT('Origin',(14.,0.,5.6));
#5431=CARTESIAN_POINT('',(0.,0.,0.));
#5432=CARTESIAN_POINT('Origin',(0.3,0.4,0.));
#5433=CARTESIAN_POINT('',(-0.3,0.4,-3.67394039744206E-17));
#5434=CARTESIAN_POINT('Origin',(0.,0.4,0.));
#5435=CARTESIAN_POINT('Origin',(0.,0.375,0.));
#5436=CARTESIAN_POINT('',(-0.35,0.35,-4.28626379701573E-17));
#5437=CARTESIAN_POINT('Origin',(0.,0.35,0.));
#5438=CARTESIAN_POINT('',(-0.325,0.375,-3.9801020972289E-17));
#5439=CARTESIAN_POINT('Origin',(0.,0.19,0.));
#5440=CARTESIAN_POINT('',(-0.35,0.03,-4.28626379701574E-17));
#5441=CARTESIAN_POINT('Origin',(0.,0.03,0.));
#5442=CARTESIAN_POINT('',(-0.35,0.19,-4.28626379701574E-17));
#5443=CARTESIAN_POINT('Origin',(0.,0.0149999999999999,0.));
#5444=CARTESIAN_POINT('',(-0.32,-3.29597460435593E-17,-3.91886975727153E-17));
#5445=CARTESIAN_POINT('Origin',(0.,0.,0.));
#5446=CARTESIAN_POINT('',(-0.335,0.0149999999999999,-4.10256677714363E-17));
#5447=CARTESIAN_POINT('Origin',(0.22,0.,0.));
#5448=CARTESIAN_POINT('',(-0.22,-6.93889390390723E-18,-2.69422295812418E-17));
#5449=CARTESIAN_POINT('Origin',(0.,0.,0.));
#5450=CARTESIAN_POINT('Origin',(0.,-0.02,0.));
#5451=CARTESIAN_POINT('',(-0.1954,-0.0492,2.39295984553393E-17));
#5452=CARTESIAN_POINT('Origin',(0.,-0.0492,0.));
#5453=CARTESIAN_POINT('',(-0.21,-0.02,-2.57175827820944E-17));
#5454=CARTESIAN_POINT('Origin',(0.,-0.8,0.));
#5455=CARTESIAN_POINT('',(-0.1954,-1.5646,2.39295984553393E-17));
#5456=CARTESIAN_POINT('Origin',(0.,-1.5646,0.));
#5457=CARTESIAN_POINT('',(-0.1954,-0.8,-2.39295984553393E-17));
#5458=CARTESIAN_POINT('Origin',(0.,-1.58,0.));
#5459=CARTESIAN_POINT('',(-0.16,-1.6,-1.95943487863577E-17));
#5460=CARTESIAN_POINT('Origin',(0.,-1.6,0.));
#5461=CARTESIAN_POINT('',(-0.18,-1.58,-2.20436423846524E-17));
#5462=CARTESIAN_POINT('Origin',(0.,-1.6,0.));
#5463=CARTESIAN_POINT('Origin',(0.0866025403784439,-0.4,-0.15));
#5464=CARTESIAN_POINT('',(0.173205080756888,-0.4,0.));
#5465=CARTESIAN_POINT('',(0.0866025403784439,-0.4,-0.15));
#5466=CARTESIAN_POINT('',(0.173205080756888,-0.4,0.));
#5467=CARTESIAN_POINT('',(0.0866025403784439,-0.64,-0.15));
#5468=CARTESIAN_POINT('',(0.0866025403784439,-0.4,-0.15));
#5469=CARTESIAN_POINT('',(0.173205080756888,-0.64,0.));
#5470=CARTESIAN_POINT('',(0.173205080756888,-0.64,0.));
#5471=CARTESIAN_POINT('',(0.173205080756888,-0.4,0.));
#5472=CARTESIAN_POINT('Origin',(-0.0866025403784438,-0.4,-0.15));
#5473=CARTESIAN_POINT('',(-0.0866025403784438,-0.4,-0.15));
#5474=CARTESIAN_POINT('',(0.0866025403784439,-0.4,-0.15));
#5475=CARTESIAN_POINT('',(-0.0866025403784438,-0.64,-0.15));
#5476=CARTESIAN_POINT('',(-0.0866025403784438,-0.4,-0.15));
#5477=CARTESIAN_POINT('',(0.0866025403784439,-0.64,-0.15));
#5478=CARTESIAN_POINT('Origin',(-0.173205080756888,-0.4,-2.77555756156289E-17));
#5479=CARTESIAN_POINT('',(-0.173205080756888,-0.4,-2.12115047744981E-17));
#5480=CARTESIAN_POINT('',(-0.0866025403784438,-0.4,-0.15));
#5481=CARTESIAN_POINT('',(-0.173205080756888,-0.64,-2.77555756156289E-17));
#5482=CARTESIAN_POINT('',(-0.173205080756888,-0.4,-2.12115047744981E-17));
#5483=CARTESIAN_POINT('',(-0.0866025403784438,-0.64,-0.15));
#5484=CARTESIAN_POINT('Origin',(-0.0866025403784439,-0.4,0.15));
#5485=CARTESIAN_POINT('',(-0.0866025403784439,-0.4,0.15));
#5486=CARTESIAN_POINT('',(-0.173205080756888,-0.4,-2.12115047744981E-17));
#5487=CARTESIAN_POINT('',(-0.0866025403784439,-0.64,0.15));
#5488=CARTESIAN_POINT('',(-0.0866025403784439,-0.4,0.15));
#5489=CARTESIAN_POINT('',(-0.173205080756888,-0.64,-2.12115047744981E-17));
#5490=CARTESIAN_POINT('Origin',(0.0866025403784439,-0.4,0.15));
#5491=CARTESIAN_POINT('',(0.0866025403784439,-0.4,0.15));
#5492=CARTESIAN_POINT('',(-0.0866025403784439,-0.4,0.15));
#5493=CARTESIAN_POINT('',(0.0866025403784439,-0.64,0.15));
#5494=CARTESIAN_POINT('',(0.0866025403784439,-0.4,0.15));
#5495=CARTESIAN_POINT('',(-0.0866025403784439,-0.64,0.15));
#5496=CARTESIAN_POINT('Origin',(0.173205080756888,-0.4,0.));
#5497=CARTESIAN_POINT('',(0.0866025403784439,-0.4,0.15));
#5498=CARTESIAN_POINT('',(0.0866025403784439,-0.64,0.15));
#5499=CARTESIAN_POINT('Origin',(0.,-0.4,-2.77555756156289E-17));
#5500=CARTESIAN_POINT('Origin',(0.,-0.64,-2.77555756156289E-17));
#5501=CARTESIAN_POINT('',(0.,0.,0.));
#5502=CARTESIAN_POINT('Origin',(0.,0.,0.));
#5503=CARTESIAN_POINT('',(-0.42,0.16,5.14351655641888E-17));
#5504=CARTESIAN_POINT('Origin',(0.,0.16,0.));
#5505=CARTESIAN_POINT('',(-0.42,0.,5.14351655641888E-17));
#5506=CARTESIAN_POINT('',(-0.42,0.,5.14351655641888E-17));
#5507=CARTESIAN_POINT('Origin',(0.,0.,0.));
#5508=CARTESIAN_POINT('Origin',(0.,0.,0.));
#5509=CARTESIAN_POINT('',(-0.8,0.16,9.79717439317883E-17));
#5510=CARTESIAN_POINT('Origin',(0.,0.16,0.));
#5511=CARTESIAN_POINT('',(-0.8,0.,9.79717439317883E-17));
#5512=CARTESIAN_POINT('',(-0.8,0.,9.79717439317883E-17));
#5513=CARTESIAN_POINT('Origin',(0.,0.,0.));
#5514=CARTESIAN_POINT('Origin',(0.,0.16,0.));
#5515=CARTESIAN_POINT('Origin',(0.,0.,0.));
#5516=CARTESIAN_POINT('',(0.,0.,0.));
#5517=CARTESIAN_POINT('',(2.5,0.,1.42));
#5518=CARTESIAN_POINT('',(2.5,0.,4.));
#5519=CARTESIAN_POINT('',(2.5,0.,4.1));
#5520=CARTESIAN_POINT('',(7.5,0.,1.42));
#5521=CARTESIAN_POINT('',(7.5,0.,4.));
#5522=CARTESIAN_POINT('',(7.5,0.,4.1));
#5523=CARTESIAN_POINT('',(0.,0.,1.));
#5524=CARTESIAN_POINT('',(5.,0.,3.04));
#5525=CARTESIAN_POINT('',(5.,0.,3.04));
#5526=CARTESIAN_POINT('',(0.,0.,0.));
#5527=CARTESIAN_POINT('Origin',(0.,0.067277284513851,0.));
#5528=CARTESIAN_POINT('',(-0.375277674973257,0.0768195421087395,0.65));
#5529=CARTESIAN_POINT('',(0.375277674973257,0.0768195421087395,0.65));
#5530=CARTESIAN_POINT('Ctrl Pts',(-0.375277674973257,0.0768195421087395,
0.65));
#5531=CARTESIAN_POINT('Ctrl Pts',(1.66533453693773E-13,-0.0315137912242439,
0.65));
#5532=CARTESIAN_POINT('Ctrl Pts',(0.375277674973257,0.0768195421087394,
0.65));
#5533=CARTESIAN_POINT('',(-0.750555349946514,0.0768195421087394,-9.19165206894919E-17));
#5534=CARTESIAN_POINT('Ctrl Pts',(-0.750555349946514,0.0768195421087394,
-9.19165206894919E-17));
#5535=CARTESIAN_POINT('Ctrl Pts',(-0.562916512459802,-0.0315137912242434,
0.325000000000144));
#5536=CARTESIAN_POINT('Ctrl Pts',(-0.375277674973257,0.0768195421087395,
0.65));
#5537=CARTESIAN_POINT('',(-0.6175,-2.77555756156289E-17,-7.5621939847349E-17));
#5538=CARTESIAN_POINT('',(-0.734027674973257,0.067277284513851,-8.98924642641573E-17));
#5539=CARTESIAN_POINT('Origin',(0.,0.,0.));
#5540=CARTESIAN_POINT('',(-0.375277674973257,0.0768195421087395,-0.65));
#5541=CARTESIAN_POINT('Ctrl Pts',(-0.375277674973257,0.0768195421087395,
-0.65));
#5542=CARTESIAN_POINT('Ctrl Pts',(-0.562916512459968,-0.0315137912242437,
-0.324999999999856));
#5543=CARTESIAN_POINT('Ctrl Pts',(-0.750555349946514,0.0768195421087395,
-9.19165206894919E-17));
#5544=CARTESIAN_POINT('',(0.375277674973257,0.0768195421087395,-0.65));
#5545=CARTESIAN_POINT('Ctrl Pts',(0.375277674973257,0.0768195421087395,
-0.65));
#5546=CARTESIAN_POINT('Ctrl Pts',(-1.66144875635155E-13,-0.0315137912242437,
-0.65));
#5547=CARTESIAN_POINT('Ctrl Pts',(-0.375277674973257,0.0768195421087395,
-0.65));
#5548=CARTESIAN_POINT('',(0.750555349946514,0.0768195421087394,0.));
#5549=CARTESIAN_POINT('Ctrl Pts',(0.750555349946514,0.0768195421087394,
0.));
#5550=CARTESIAN_POINT('Ctrl Pts',(0.562916512459802,-0.0315137912242436,
-0.325000000000144));
#5551=CARTESIAN_POINT('Ctrl Pts',(0.375277674973257,0.0768195421087395,
-0.65));
#5552=CARTESIAN_POINT('Ctrl Pts',(0.375277674973257,0.0768195421087394,
0.65));
#5553=CARTESIAN_POINT('Ctrl Pts',(0.562916512459968,-0.0315137912242439,
0.324999999999856));
#5554=CARTESIAN_POINT('Ctrl Pts',(0.750555349946514,0.0768195421087394,
0.));
#5555=CARTESIAN_POINT('Origin',(0.,0.612722715486149,0.));
#5556=CARTESIAN_POINT('',(-0.6175,0.68,-7.5621939847349E-17));
#5557=CARTESIAN_POINT('Origin',(0.,0.68,0.));
#5558=CARTESIAN_POINT('',(-0.750555349946514,0.603180457891261,-9.19165206894919E-17));
#5559=CARTESIAN_POINT('',(-0.734027674973257,0.612722715486149,-8.98924642641573E-17));
#5560=CARTESIAN_POINT('',(-0.375277674973257,0.603180457891261,0.65));
#5561=CARTESIAN_POINT('Ctrl Pts',(-0.375277674973257,0.603180457891261,
0.65));
#5562=CARTESIAN_POINT('Ctrl Pts',(-0.562916512459968,0.711513791224243,
0.324999999999856));
#5563=CARTESIAN_POINT('Ctrl Pts',(-0.750555349946514,0.603180457891261,
-9.19165206894919E-17));
#5564=CARTESIAN_POINT('',(0.375277674973257,0.603180457891261,0.65));
#5565=CARTESIAN_POINT('Ctrl Pts',(0.375277674973257,0.603180457891261,0.65));
#5566=CARTESIAN_POINT('Ctrl Pts',(-1.66755498298699E-13,0.711513791224244,
0.65));
#5567=CARTESIAN_POINT('Ctrl Pts',(-0.375277674973257,0.603180457891261,
0.65));
#5568=CARTESIAN_POINT('',(0.750555349946514,0.603180457891261,0.));
#5569=CARTESIAN_POINT('Ctrl Pts',(0.750555349946514,0.603180457891261,0.));
#5570=CARTESIAN_POINT('Ctrl Pts',(0.562916512459802,0.711513791224244,0.325000000000144));
#5571=CARTESIAN_POINT('Ctrl Pts',(0.375277674973257,0.603180457891261,0.65));
#5572=CARTESIAN_POINT('',(0.375277674973257,0.603180457891261,-0.65));
#5573=CARTESIAN_POINT('Ctrl Pts',(0.375277674973257,0.603180457891261,-0.65));
#5574=CARTESIAN_POINT('Ctrl Pts',(0.562916512459969,0.711513791224244,-0.324999999999856));
#5575=CARTESIAN_POINT('Ctrl Pts',(0.750555349946514,0.603180457891261,0.));
#5576=CARTESIAN_POINT('',(-0.375277674973257,0.603180457891261,-0.65));
#5577=CARTESIAN_POINT('Ctrl Pts',(-0.375277674973257,0.603180457891261,
-0.65));
#5578=CARTESIAN_POINT('Ctrl Pts',(1.66422431391311E-13,0.711513791224244,
-0.65));
#5579=CARTESIAN_POINT('Ctrl Pts',(0.375277674973257,0.603180457891261,-0.65));
#5580=CARTESIAN_POINT('Ctrl Pts',(-0.750555349946514,0.603180457891261,
-9.19165206894919E-17));
#5581=CARTESIAN_POINT('Ctrl Pts',(-0.562916512459802,0.711513791224244,
-0.325000000000144));
#5582=CARTESIAN_POINT('Ctrl Pts',(-0.375277674973257,0.603180457891261,
-0.65));
#5583=CARTESIAN_POINT('Origin',(0.375277674973257,0.,-0.65));
#5584=CARTESIAN_POINT('',(-0.375277674973257,0.,-0.65));
#5585=CARTESIAN_POINT('',(0.375277674973257,0.,-0.65));
#5586=CARTESIAN_POINT('Origin',(-0.375277674973257,0.,-0.65));
#5587=CARTESIAN_POINT('',(-0.750555349946514,0.,-9.19165206894919E-17));
#5588=CARTESIAN_POINT('Origin',(-0.750555349946514,0.,-9.19165206894919E-17));
#5589=CARTESIAN_POINT('',(-0.375277674973257,0.,0.65));
#5590=CARTESIAN_POINT('Origin',(0.,0.,0.));
#5591=CARTESIAN_POINT('',(-0.338975,0.68,4.15124648740974E-17));
#5592=CARTESIAN_POINT('Origin',(0.,0.68,0.));
#5593=CARTESIAN_POINT('',(-0.338975,0.,4.15124648740974E-17));
#5594=CARTESIAN_POINT('',(-0.338975,0.,4.15124648740974E-17));
#5595=CARTESIAN_POINT('Origin',(0.,0.,0.));
#5596=CARTESIAN_POINT('Origin',(-0.375277674973257,0.,0.65));
#5597=CARTESIAN_POINT('',(0.375277674973257,0.,0.65));
#5598=CARTESIAN_POINT('Origin',(0.750555349946514,0.,0.));
#5599=CARTESIAN_POINT('',(0.750555349946514,0.,0.));
#5600=CARTESIAN_POINT('Origin',(0.375277674973257,0.,0.65));
#5601=CARTESIAN_POINT('Origin',(0.,0.68,-1.11022302462516E-16));
#5602=CARTESIAN_POINT('Origin',(0.,0.,-1.11022302462516E-16));
#5603=CARTESIAN_POINT('',(0.,0.,0.));
#5604=CARTESIAN_POINT('Origin',(6.5,-5.73205080756888,7.22132034));
#5605=CARTESIAN_POINT('',(6.89841665441537,-5.69649564641799,8.48132034));
#5606=CARTESIAN_POINT('',(6.89841665441537,-5.69649564641799,7.28132034));
#5607=CARTESIAN_POINT('',(6.89841665441537,-5.69649564641799,7.22132034));
#5608=CARTESIAN_POINT('',(6.33158334558463,-5.36923428297892,8.48132034));
#5609=CARTESIAN_POINT('Origin',(6.5,-5.73205080756888,8.48132034));
#5610=CARTESIAN_POINT('',(6.33158334558463,-5.36923428297892,7.28132034));
#5611=CARTESIAN_POINT('',(6.33158334558463,-5.36923428297892,7.22132034));
#5612=CARTESIAN_POINT('Origin',(6.5,-5.73205080756888,7.28132034));
#5613=CARTESIAN_POINT('Origin',(9.5,-4.,7.22132034));
#5614=CARTESIAN_POINT('',(9.27,-4.32726136343907,7.28132034));
#5615=CARTESIAN_POINT('',(9.27,-4.32726136343907,8.48132034));
#5616=CARTESIAN_POINT('',(9.27,-4.32726136343907,7.22132034));
#5617=CARTESIAN_POINT('',(9.27,-3.67273863656093,7.28132034));
#5618=CARTESIAN_POINT('Origin',(9.5,-4.,7.28132034));
#5619=CARTESIAN_POINT('',(9.27,-3.67273863656093,8.48132034));
#5620=CARTESIAN_POINT('',(9.27,-3.67273863656093,7.22132034));
#5621=CARTESIAN_POINT('Origin',(9.5,-4.,8.48132034));
#5622=CARTESIAN_POINT('Origin',(8.5,-2.26794919243112,7.22132034));
#5623=CARTESIAN_POINT('',(8.10158334558463,-2.30350435358201,8.48132034));
#5624=CARTESIAN_POINT('',(8.10158334558463,-2.30350435358201,7.28132034));
#5625=CARTESIAN_POINT('',(8.10158334558463,-2.30350435358201,7.22132034));
#5626=CARTESIAN_POINT('',(8.66841665441537,-2.63076571702108,8.48132034));
#5627=CARTESIAN_POINT('Origin',(8.5,-2.26794919243112,8.48132034));
#5628=CARTESIAN_POINT('',(8.66841665441537,-2.63076571702108,7.28132034));
#5629=CARTESIAN_POINT('',(8.66841665441537,-2.63076571702108,7.22132034));
#5630=CARTESIAN_POINT('Origin',(8.5,-2.26794919243112,7.28132034));
#5631=CARTESIAN_POINT('Origin',(6.5,-2.26794919243112,7.22132034));
#5632=CARTESIAN_POINT('',(6.33158334558463,-2.63076571702108,8.48132034));
#5633=CARTESIAN_POINT('',(6.33158334558463,-2.63076571702108,7.28132034));
#5634=CARTESIAN_POINT('',(6.33158334558463,-2.63076571702108,7.22132034));
#5635=CARTESIAN_POINT('',(6.89841665441537,-2.30350435358201,8.48132034));
#5636=CARTESIAN_POINT('Origin',(6.5,-2.26794919243112,8.48132034));
#5637=CARTESIAN_POINT('',(6.89841665441537,-2.30350435358201,7.28132034));
#5638=CARTESIAN_POINT('',(6.89841665441537,-2.30350435358201,7.22132034));
#5639=CARTESIAN_POINT('Origin',(6.5,-2.26794919243112,7.28132034));
#5640=CARTESIAN_POINT('Origin',(5.5,-4.,7.22132034));
#5641=CARTESIAN_POINT('',(5.73,-4.32726136343907,8.48132034));
#5642=CARTESIAN_POINT('',(5.73,-4.32726136343907,7.28132034));
#5643=CARTESIAN_POINT('',(5.73,-4.32726136343907,7.22132034));
#5644=CARTESIAN_POINT('',(5.73,-3.67273863656093,8.48132034));
#5645=CARTESIAN_POINT('Origin',(5.5,-4.,8.48132034));
#5646=CARTESIAN_POINT('',(5.73,-3.67273863656093,7.28132034));
#5647=CARTESIAN_POINT('',(5.73,-3.67273863656093,7.22132034));
#5648=CARTESIAN_POINT('Origin',(5.5,-4.,7.28132034));
#5649=CARTESIAN_POINT('Origin',(8.5,-5.73205080756888,7.22132034));
#5650=CARTESIAN_POINT('',(8.66841665441537,-5.36923428297892,8.48132034));
#5651=CARTESIAN_POINT('',(8.66841665441537,-5.36923428297892,7.28132034));
#5652=CARTESIAN_POINT('',(8.66841665441537,-5.36923428297892,7.22132034));
#5653=CARTESIAN_POINT('',(8.10158334558463,-5.69649564641799,8.48132034));
#5654=CARTESIAN_POINT('Origin',(8.5,-5.73205080756888,8.48132034));
#5655=CARTESIAN_POINT('',(8.10158334558463,-5.69649564641799,7.28132034));
#5656=CARTESIAN_POINT('',(8.10158334558463,-5.69649564641799,7.22132034));
#5657=CARTESIAN_POINT('Origin',(8.5,-5.73205080756888,7.28132034));
#5658=CARTESIAN_POINT('Origin',(7.5,-4.,8.48132034));
#5659=CARTESIAN_POINT('Origin',(7.5,-4.,8.48132034));
#5660=CARTESIAN_POINT('Origin',(7.5,-4.,8.48132034));
#5661=CARTESIAN_POINT('Origin',(7.5,-4.,8.48132034));
#5662=CARTESIAN_POINT('Origin',(7.5,-4.,8.48132034));
#5663=CARTESIAN_POINT('Origin',(7.5,-4.,8.48132034));
#5664=CARTESIAN_POINT('Origin',(7.5,-4.,8.48132034));
#5665=CARTESIAN_POINT('',(7.075,-4.,8.48132034));
#5666=CARTESIAN_POINT('Origin',(7.5,-4.,8.48132034));
#5667=CARTESIAN_POINT('Origin',(7.5,-4.,7.28132034));
#5668=CARTESIAN_POINT('Origin',(7.5,-4.,7.28132034));
#5669=CARTESIAN_POINT('Origin',(7.5,-4.,7.28132034));
#5670=CARTESIAN_POINT('Origin',(7.5,-4.,7.28132034));
#5671=CARTESIAN_POINT('Origin',(7.5,-4.,7.28132034));
#5672=CARTESIAN_POINT('Origin',(7.5,-4.,7.28132034));
#5673=CARTESIAN_POINT('Origin',(7.5,-4.,7.28132034));
#5674=CARTESIAN_POINT('Origin',(7.5,-4.,7.28132034));
#5675=CARTESIAN_POINT('Origin',(7.5,-4.,7.28132034));
#5676=CARTESIAN_POINT('Origin',(7.5,-4.,7.28132034));
#5677=CARTESIAN_POINT('Origin',(7.5,-4.,7.28132034));
#5678=CARTESIAN_POINT('Origin',(7.5,-4.,7.28132034));
#5679=CARTESIAN_POINT('Origin',(7.87527767497326,-3.35,7.27132034));
#5680=CARTESIAN_POINT('',(7.87527767497326,-3.35,7.28132034));
#5681=CARTESIAN_POINT('',(7.12472232502674,-3.35,7.28132034));
#5682=CARTESIAN_POINT('',(7.68763883748663,-3.35,7.28132034));
#5683=CARTESIAN_POINT('',(7.87527767497326,-3.35,7.97132034));
#5684=CARTESIAN_POINT('',(7.87527767497326,-3.35,7.27132034));
#5685=CARTESIAN_POINT('',(7.12472232502674,-3.35,7.97132034));
#5686=CARTESIAN_POINT('',(7.87527767497326,-3.35,7.97132034));
#5687=CARTESIAN_POINT('',(7.12472232502674,-3.35,7.27132034));
#5688=CARTESIAN_POINT('Origin',(7.12472232502674,-3.35,7.27132034));
#5689=CARTESIAN_POINT('',(6.74944465005349,-4.,7.28132034));
#5690=CARTESIAN_POINT('',(7.03090290628343,-3.5125,7.28132034));
#5691=CARTESIAN_POINT('',(6.74944465005349,-4.,7.97132034));
#5692=CARTESIAN_POINT('',(7.12472232502674,-3.35,7.97132034));
#5693=CARTESIAN_POINT('',(6.74944465005349,-4.,7.27132034));
#5694=CARTESIAN_POINT('Origin',(6.74944465005349,-4.,7.27132034));
#5695=CARTESIAN_POINT('',(7.12472232502674,-4.65,7.28132034));
#5696=CARTESIAN_POINT('',(6.8432640687968,-4.1625,7.28132034));
#5697=CARTESIAN_POINT('',(7.12472232502674,-4.65,7.97132034));
#5698=CARTESIAN_POINT('',(6.74944465005349,-4.,7.97132034));
#5699=CARTESIAN_POINT('',(7.12472232502674,-4.65,7.27132034));
#5700=CARTESIAN_POINT('Origin',(7.12472232502674,-4.65,7.27132034));
#5701=CARTESIAN_POINT('',(7.87527767497326,-4.65,7.28132034));
#5702=CARTESIAN_POINT('',(7.31236116251337,-4.65,7.28132034));
#5703=CARTESIAN_POINT('',(7.87527767497326,-4.65,7.97132034));
#5704=CARTESIAN_POINT('',(7.12472232502674,-4.65,7.97132034));
#5705=CARTESIAN_POINT('',(7.87527767497326,-4.65,7.27132034));
#5706=CARTESIAN_POINT('Origin',(8.25055534994651,-4.,7.27132034));
#5707=CARTESIAN_POINT('',(8.25055534994651,-4.,7.28132034));
#5708=CARTESIAN_POINT('',(8.1567359312032,-3.8375,7.28132034));
#5709=CARTESIAN_POINT('',(8.25055534994651,-4.,7.97132034));
#5710=CARTESIAN_POINT('',(8.25055534994651,-4.,7.27132034));
#5711=CARTESIAN_POINT('',(8.25055534994651,-4.,7.97132034));
#5712=CARTESIAN_POINT('Origin',(7.87527767497326,-4.65,7.27132034));
#5713=CARTESIAN_POINT('',(7.96909709371657,-4.4875,7.28132034));
#5714=CARTESIAN_POINT('',(7.87527767497326,-4.65,7.97132034));
#5715=CARTESIAN_POINT('Origin',(7.5,-4.,7.97132034));
#5716=CARTESIAN_POINT('',(7.075,-4.,7.97132034));
#5717=CARTESIAN_POINT('Origin',(7.5,-4.,7.97132034));
#5718=CARTESIAN_POINT('Origin',(7.5,-4.,7.28132034));
#5719=CARTESIAN_POINT('',(7.075,-4.,7.28132034));
#5720=CARTESIAN_POINT('Origin',(7.5,-4.,7.28132034));
#5721=CARTESIAN_POINT('',(0.,0.,0.));
#5722=CARTESIAN_POINT('',(0.,0.,0.));
#5723=CARTESIAN_POINT('',(14.,-0.6,6.4));
#5724=CARTESIAN_POINT('',(14.,0.6,6.4));
#5725=CARTESIAN_POINT('',(5.,0.,5.6));
#5726=CARTESIAN_POINT('',(5.,0.,5.76));
#5727=CARTESIAN_POINT('',(-2.5,4.,-1.52132034355964));
#5728=CARTESIAN_POINT('',(0.,0.,0.));
#5729=CARTESIAN_POINT('',(1.22807019788979,-3.28215562823474,-1.71914004176867E-15));
#5730=UNCERTAINTY_MEASURE_WITH_UNIT(LENGTH_MEASURE(0.001),#5762,
'DISTANCE_ACCURACY_VALUE',
'Maximum model space distance between geometric entities at asserted c
onnectivities');
#5731=UNCERTAINTY_MEASURE_WITH_UNIT(LENGTH_MEASURE(0.001),#5762,
'DISTANCE_ACCURACY_VALUE',
'Maximum model space distance between geometric entities at asserted c
onnectivities');
#5732=UNCERTAINTY_MEASURE_WITH_UNIT(LENGTH_MEASURE(0.001),#5762,
'DISTANCE_ACCURACY_VALUE',
'Maximum model space distance between geometric entities at asserted c
onnectivities');
#5733=UNCERTAINTY_MEASURE_WITH_UNIT(LENGTH_MEASURE(0.001),#5762,
'DISTANCE_ACCURACY_VALUE',
'Maximum model space distance between geometric entities at asserted c
onnectivities');
#5734=UNCERTAINTY_MEASURE_WITH_UNIT(LENGTH_MEASURE(0.001),#5762,
'DISTANCE_ACCURACY_VALUE',
'Maximum model space distance between geometric entities at asserted c
onnectivities');
#5735=UNCERTAINTY_MEASURE_WITH_UNIT(LENGTH_MEASURE(0.001),#5762,
'DISTANCE_ACCURACY_VALUE',
'Maximum model space distance between geometric entities at asserted c
onnectivities');
#5736=UNCERTAINTY_MEASURE_WITH_UNIT(LENGTH_MEASURE(0.001),#5762,
'DISTANCE_ACCURACY_VALUE',
'Maximum model space distance between geometric entities at asserted c
onnectivities');
#5737=UNCERTAINTY_MEASURE_WITH_UNIT(LENGTH_MEASURE(0.001),#5762,
'DISTANCE_ACCURACY_VALUE',
'Maximum model space distance between geometric entities at asserted c
onnectivities');
#5738=UNCERTAINTY_MEASURE_WITH_UNIT(LENGTH_MEASURE(0.001),#5762,
'DISTANCE_ACCURACY_VALUE',
'Maximum model space distance between geometric entities at asserted c
onnectivities');
#5739=UNCERTAINTY_MEASURE_WITH_UNIT(LENGTH_MEASURE(0.001),#5762,
'DISTANCE_ACCURACY_VALUE',
'Maximum model space distance between geometric entities at asserted c
onnectivities');
#5740=UNCERTAINTY_MEASURE_WITH_UNIT(LENGTH_MEASURE(0.001),#5762,
'DISTANCE_ACCURACY_VALUE',
'Maximum model space distance between geometric entities at asserted c
onnectivities');
#5741=UNCERTAINTY_MEASURE_WITH_UNIT(LENGTH_MEASURE(0.001),#5762,
'DISTANCE_ACCURACY_VALUE',
'Maximum model space distance between geometric entities at asserted c
onnectivities');
#5742=UNCERTAINTY_MEASURE_WITH_UNIT(LENGTH_MEASURE(0.001),#5762,
'DISTANCE_ACCURACY_VALUE',
'Maximum model space distance between geometric entities at asserted c
onnectivities');
#5743=UNCERTAINTY_MEASURE_WITH_UNIT(LENGTH_MEASURE(0.001),#5762,
'DISTANCE_ACCURACY_VALUE',
'Maximum model space distance between geometric entities at asserted c
onnectivities');
#5744=UNCERTAINTY_MEASURE_WITH_UNIT(LENGTH_MEASURE(0.001),#5762,
'DISTANCE_ACCURACY_VALUE',
'Maximum model space distance between geometric entities at asserted c
onnectivities');
#5745=UNCERTAINTY_MEASURE_WITH_UNIT(LENGTH_MEASURE(0.001),#5762,
'DISTANCE_ACCURACY_VALUE',
'Maximum model space distance between geometric entities at asserted c
onnectivities');
#5746=(
GEOMETRIC_REPRESENTATION_CONTEXT(3)
GLOBAL_UNCERTAINTY_ASSIGNED_CONTEXT((#5730))
GLOBAL_UNIT_ASSIGNED_CONTEXT((#5762,#5764,#5765))
REPRESENTATION_CONTEXT('','3D')
);
#5747=(
GEOMETRIC_REPRESENTATION_CONTEXT(3)
GLOBAL_UNCERTAINTY_ASSIGNED_CONTEXT((#5731))
GLOBAL_UNIT_ASSIGNED_CONTEXT((#5762,#5764,#5765))
REPRESENTATION_CONTEXT('','3D')
);
#5748=(
GEOMETRIC_REPRESENTATION_CONTEXT(3)
GLOBAL_UNCERTAINTY_ASSIGNED_CONTEXT((#5732))
GLOBAL_UNIT_ASSIGNED_CONTEXT((#5762,#5764,#5765))
REPRESENTATION_CONTEXT('','3D')
);
#5749=(
GEOMETRIC_REPRESENTATION_CONTEXT(3)
GLOBAL_UNCERTAINTY_ASSIGNED_CONTEXT((#5733))
GLOBAL_UNIT_ASSIGNED_CONTEXT((#5762,#5764,#5765))
REPRESENTATION_CONTEXT('','3D')
);
#5750=(
GEOMETRIC_REPRESENTATION_CONTEXT(3)
GLOBAL_UNCERTAINTY_ASSIGNED_CONTEXT((#5734))
GLOBAL_UNIT_ASSIGNED_CONTEXT((#5762,#5764,#5765))
REPRESENTATION_CONTEXT('','3D')
);
#5751=(
GEOMETRIC_REPRESENTATION_CONTEXT(3)
GLOBAL_UNCERTAINTY_ASSIGNED_CONTEXT((#5735))
GLOBAL_UNIT_ASSIGNED_CONTEXT((#5762,#5764,#5765))
REPRESENTATION_CONTEXT('','3D')
);
#5752=(
GEOMETRIC_REPRESENTATION_CONTEXT(3)
GLOBAL_UNCERTAINTY_ASSIGNED_CONTEXT((#5736))
GLOBAL_UNIT_ASSIGNED_CONTEXT((#5762,#5764,#5765))
REPRESENTATION_CONTEXT('','3D')
);
#5753=(
GEOMETRIC_REPRESENTATION_CONTEXT(3)
GLOBAL_UNCERTAINTY_ASSIGNED_CONTEXT((#5737))
GLOBAL_UNIT_ASSIGNED_CONTEXT((#5762,#5764,#5765))
REPRESENTATION_CONTEXT('','3D')
);
#5754=(
GEOMETRIC_REPRESENTATION_CONTEXT(3)
GLOBAL_UNCERTAINTY_ASSIGNED_CONTEXT((#5738))
GLOBAL_UNIT_ASSIGNED_CONTEXT((#5762,#5764,#5765))
REPRESENTATION_CONTEXT('','3D')
);
#5755=(
GEOMETRIC_REPRESENTATION_CONTEXT(3)
GLOBAL_UNCERTAINTY_ASSIGNED_CONTEXT((#5739))
GLOBAL_UNIT_ASSIGNED_CONTEXT((#5762,#5764,#5765))
REPRESENTATION_CONTEXT('','3D')
);
#5756=(
GEOMETRIC_REPRESENTATION_CONTEXT(3)
GLOBAL_UNCERTAINTY_ASSIGNED_CONTEXT((#5740))
GLOBAL_UNIT_ASSIGNED_CONTEXT((#5762,#5764,#5765))
REPRESENTATION_CONTEXT('','3D')
);
#5757=(
GEOMETRIC_REPRESENTATION_CONTEXT(3)
GLOBAL_UNCERTAINTY_ASSIGNED_CONTEXT((#5741))
GLOBAL_UNIT_ASSIGNED_CONTEXT((#5762,#5764,#5765))
REPRESENTATION_CONTEXT('','3D')
);
#5758=(
GEOMETRIC_REPRESENTATION_CONTEXT(3)
GLOBAL_UNCERTAINTY_ASSIGNED_CONTEXT((#5742))
GLOBAL_UNIT_ASSIGNED_CONTEXT((#5762,#5764,#5765))
REPRESENTATION_CONTEXT('','3D')
);
#5759=(
GEOMETRIC_REPRESENTATION_CONTEXT(3)
GLOBAL_UNCERTAINTY_ASSIGNED_CONTEXT((#5743))
GLOBAL_UNIT_ASSIGNED_CONTEXT((#5762,#5764,#5765))
REPRESENTATION_CONTEXT('','3D')
);
#5760=(
GEOMETRIC_REPRESENTATION_CONTEXT(3)
GLOBAL_UNCERTAINTY_ASSIGNED_CONTEXT((#5744))
GLOBAL_UNIT_ASSIGNED_CONTEXT((#5762,#5764,#5765))
REPRESENTATION_CONTEXT('','3D')
);
#5761=(
GEOMETRIC_REPRESENTATION_CONTEXT(3)
GLOBAL_UNCERTAINTY_ASSIGNED_CONTEXT((#5745))
GLOBAL_UNIT_ASSIGNED_CONTEXT((#5762,#5764,#5765))
REPRESENTATION_CONTEXT('','3D')
);
#5762=(
LENGTH_UNIT()
NAMED_UNIT(*)
SI_UNIT(.CENTI.,.METRE.)
);
#5763=(
LENGTH_UNIT()
NAMED_UNIT(*)
SI_UNIT($,.METRE.)
);
#5764=(
NAMED_UNIT(*)
PLANE_ANGLE_UNIT()
SI_UNIT($,.RADIAN.)
);
#5765=(
NAMED_UNIT(*)
SI_UNIT($,.STERADIAN.)
SOLID_ANGLE_UNIT()
);
#5766=SHAPE_DEFINITION_REPRESENTATION(#5781,#5815);
#5767=SHAPE_DEFINITION_REPRESENTATION(#5782,#5816);
#5768=SHAPE_DEFINITION_REPRESENTATION(#5783,#5817);
#5769=SHAPE_DEFINITION_REPRESENTATION(#5784,#5818);
#5770=SHAPE_DEFINITION_REPRESENTATION(#5785,#5819);
#5771=SHAPE_DEFINITION_REPRESENTATION(#5786,#5820);
#5772=SHAPE_DEFINITION_REPRESENTATION(#5787,#5821);
#5773=SHAPE_DEFINITION_REPRESENTATION(#5788,#5822);
#5774=SHAPE_DEFINITION_REPRESENTATION(#5789,#5823);
#5775=SHAPE_DEFINITION_REPRESENTATION(#5790,#5824);
#5776=SHAPE_DEFINITION_REPRESENTATION(#5791,#5825);
#5777=SHAPE_DEFINITION_REPRESENTATION(#5792,#5826);
#5778=SHAPE_DEFINITION_REPRESENTATION(#5793,#5827);
#5779=SHAPE_DEFINITION_REPRESENTATION(#5804,#5828);
#5780=SHAPE_DEFINITION_REPRESENTATION(#5805,#5829);
#5781=PRODUCT_DEFINITION_SHAPE('',$,#5831);
#5782=PRODUCT_DEFINITION_SHAPE('',$,#5832);
#5783=PRODUCT_DEFINITION_SHAPE('',$,#5833);
#5784=PRODUCT_DEFINITION_SHAPE('',$,#5834);
#5785=PRODUCT_DEFINITION_SHAPE('',$,#5835);
#5786=PRODUCT_DEFINITION_SHAPE('',$,#5836);
#5787=PRODUCT_DEFINITION_SHAPE('',$,#5837);
#5788=PRODUCT_DEFINITION_SHAPE('',$,#5838);
#5789=PRODUCT_DEFINITION_SHAPE('',$,#5839);
#5790=PRODUCT_DEFINITION_SHAPE('',$,#5840);
#5791=PRODUCT_DEFINITION_SHAPE('',$,#5841);
#5792=PRODUCT_DEFINITION_SHAPE('',$,#5842);
#5793=PRODUCT_DEFINITION_SHAPE('',$,#5843);
#5794=PRODUCT_DEFINITION_SHAPE($,$,#68);
#5795=PRODUCT_DEFINITION_SHAPE($,$,#69);
#5796=PRODUCT_DEFINITION_SHAPE($,$,#70);
#5797=PRODUCT_DEFINITION_SHAPE($,$,#71);
#5798=PRODUCT_DEFINITION_SHAPE($,$,#72);
#5799=PRODUCT_DEFINITION_SHAPE($,$,#73);
#5800=PRODUCT_DEFINITION_SHAPE($,$,#74);
#5801=PRODUCT_DEFINITION_SHAPE($,$,#75);
#5802=PRODUCT_DEFINITION_SHAPE($,$,#76);
#5803=PRODUCT_DEFINITION_SHAPE($,$,#77);
#5804=PRODUCT_DEFINITION_SHAPE('',$,#5844);
#5805=PRODUCT_DEFINITION_SHAPE('',$,#5845);
#5806=PRODUCT_DEFINITION_SHAPE($,$,#78);
#5807=PRODUCT_DEFINITION_SHAPE($,$,#79);
#5808=PRODUCT_DEFINITION_SHAPE($,$,#80);
#5809=PRODUCT_DEFINITION_SHAPE($,$,#81);
#5810=PRODUCT_DEFINITION_SHAPE($,$,#82);
#5811=PRODUCT_DEFINITION_SHAPE($,$,#83);
#5812=PRODUCT_DEFINITION_SHAPE($,$,#84);
#5813=PRODUCT_DEFINITION_SHAPE($,$,#85);
#5814=PRODUCT_DEFINITION_SHAPE($,$,#86);
#5815=SHAPE_REPRESENTATION('',(#3468,#3785,#3786),#5746);
#5816=SHAPE_REPRESENTATION('',(#3469,#3703,#3704,#3705,#3706,#3707,#3708,
#3709,#3710,#3711,#3712),#5747);
#5817=SHAPE_REPRESENTATION('',(#3470),#5748);
#5818=SHAPE_REPRESENTATION('',(#3498),#5749);
#5819=SHAPE_REPRESENTATION('',(#3519),#5750);
#5820=SHAPE_REPRESENTATION('',(#3530),#5751);
#5821=SHAPE_REPRESENTATION('',(#3558),#5752);
#5822=SHAPE_REPRESENTATION('',(#3608),#5753);
#5823=SHAPE_REPRESENTATION('',(#3625,#3778,#3779,#3780,#3781,#3782,#3783,
#3784),#5754);
#5824=SHAPE_REPRESENTATION('',(#3626),#5755);
#5825=SHAPE_REPRESENTATION('',(#3647),#5756);
#5826=SHAPE_REPRESENTATION('',(#3668),#5757);
#5827=SHAPE_REPRESENTATION('',(#3694),#5758);
#5828=SHAPE_REPRESENTATION('',(#3713),#5759);
#5829=SHAPE_REPRESENTATION('',(#3729),#5760);
#5830=PRODUCT_DEFINITION_CONTEXT('part definition',#5877,'design');
#5831=PRODUCT_DEFINITION('PAT-003',
'PAT-003',#5846,#5830);
#5832=PRODUCT_DEFINITION('Rail assembly','Rail assembly',#5847,
#5830);
#5833=PRODUCT_DEFINITION('Rail mounting bracket',
'Rail mounting bracket',#5848,#5830);
#5834=PRODUCT_DEFINITION('Captive slot nut','Captive slot nut',#5849,#5830);
#5835=PRODUCT_DEFINITION('Flat Washer - M5','Flat Washer - M5',#5850,#5830);
#5836=PRODUCT_DEFINITION('M5x26 bracket screw','M5x26 bracket screw',#5851,
#5830);
#5837=PRODUCT_DEFINITION('Slotted Extrusion - 20 x 20 x 100 mm',
'Slotted Extrusion - 20 x 20 x 100 mm',#5852,#5830);
#5838=PRODUCT_DEFINITION('Hex Bolt - M8x40','Hex Bolt - M8x40',#5853,#5830);
#5839=PRODUCT_DEFINITION('Swivel arm guide assembly',
'Swivel arm guide assembly',#5854,#5830);
#5840=PRODUCT_DEFINITION('Swivel guide arm','Swivel guide arm',#5855,#5830);
#5841=PRODUCT_DEFINITION('Guide contact pad','Guide contact pad',#5856,
#5830);
#5842=PRODUCT_DEFINITION('Cap Screw - M4x16','Cap Screw - M4x16',#5857,
#5830);
#5843=PRODUCT_DEFINITION('Flat Washer - M8','Flat Washer - M8',#5858,#5830);
#5844=PRODUCT_DEFINITION('Hex Nut - M8','Hex Nut - M8',#5859,#5830);
#5845=PRODUCT_DEFINITION('Captive-nut hand knob',
'Captive-nut hand knob',#5860,#5830);
#5846=PRODUCT_DEFINITION_FORMATION('',$,#5879);
#5847=PRODUCT_DEFINITION_FORMATION('',$,#5880);
#5848=PRODUCT_DEFINITION_FORMATION('',$,#5881);
#5849=PRODUCT_DEFINITION_FORMATION('',$,#5882);
#5850=PRODUCT_DEFINITION_FORMATION('',$,#5883);
#5851=PRODUCT_DEFINITION_FORMATION('',$,#5884);
#5852=PRODUCT_DEFINITION_FORMATION('',$,#5885);
#5853=PRODUCT_DEFINITION_FORMATION('',$,#5886);
#5854=PRODUCT_DEFINITION_FORMATION('',$,#5887);
#5855=PRODUCT_DEFINITION_FORMATION('',$,#5888);
#5856=PRODUCT_DEFINITION_FORMATION('',$,#5889);
#5857=PRODUCT_DEFINITION_FORMATION('',$,#5890);
#5858=PRODUCT_DEFINITION_FORMATION('',$,#5891);
#5859=PRODUCT_DEFINITION_FORMATION('',$,#5892);
#5860=PRODUCT_DEFINITION_FORMATION('',$,#5893);
#5861=PRODUCT_RELATED_PRODUCT_CATEGORY('PAT-003',
'PAT-003',(#5879));
#5862=PRODUCT_RELATED_PRODUCT_CATEGORY('Rail assembly','Rail assembly',
(#5880));
#5863=PRODUCT_RELATED_PRODUCT_CATEGORY('Rail mounting bracket',
'Rail mounting bracket',(#5881));
#5864=PRODUCT_RELATED_PRODUCT_CATEGORY('Captive slot nut',
'Captive slot nut',(#5882));
#5865=PRODUCT_RELATED_PRODUCT_CATEGORY('Flat Washer - M5',
'Flat Washer - M5',(#5883));
#5866=PRODUCT_RELATED_PRODUCT_CATEGORY('M5x26 bracket screw',
'M5x26 bracket screw',(#5884));
#5867=PRODUCT_RELATED_PRODUCT_CATEGORY(
'Slotted Extrusion - 20 x 20 x 100 mm',
'Slotted Extrusion - 20 x 20 x 100 mm',(#5885));
#5868=PRODUCT_RELATED_PRODUCT_CATEGORY('Hex Bolt - M8x40',
'Hex Bolt - M8x40',(#5886));
#5869=PRODUCT_RELATED_PRODUCT_CATEGORY('Swivel arm guide assembly',
'Swivel arm guide assembly',(#5887));
#5870=PRODUCT_RELATED_PRODUCT_CATEGORY('Swivel guide arm',
'Swivel guide arm',(#5888));
#5871=PRODUCT_RELATED_PRODUCT_CATEGORY('Guide contact pad',
'Guide contact pad',(#5889));
#5872=PRODUCT_RELATED_PRODUCT_CATEGORY('Cap Screw - M4x16',
'Cap Screw - M4x16',(#5890));
#5873=PRODUCT_RELATED_PRODUCT_CATEGORY('Flat Washer - M8',
'Flat Washer - M8',(#5891));
#5874=PRODUCT_RELATED_PRODUCT_CATEGORY('Hex Nut - M8','Hex Nut - M8',(#5892));
#5875=PRODUCT_RELATED_PRODUCT_CATEGORY('Captive-nut hand knob',
'Captive-nut hand knob',(#5893));
#5876=APPLICATION_PROTOCOL_DEFINITION('international standard',
'automotive_design',2009,#5877);
#5877=APPLICATION_CONTEXT(
'Core Data for Automotive Mechanical Design Process');
#5878=PRODUCT_CONTEXT('part definition',#5877,'mechanical');
#5879=PRODUCT('PAT-003',
'PAT-003','PAT-003',(#5878));
#5880=PRODUCT('Rail assembly','Rail assembly',
'Rail assembly',(#5878));
#5881=PRODUCT('Rail mounting bracket','Rail mounting bracket',
'Rail mounting bracket',(#5878));
#5882=PRODUCT('Captive slot nut','Captive slot nut','Captive slot nut',
(#5878));
#5883=PRODUCT('Flat Washer - M5','Flat Washer - M5','Flat Washer - M5',
(#5878));
#5884=PRODUCT('M5x26 bracket screw','M5x26 bracket screw',
'M5x26 bracket screw',(#5878));
#5885=PRODUCT('Slotted Extrusion - 20 x 20 x 100 mm',
'Slotted Extrusion - 20 x 20 x 100 mm',
'Slotted Extrusion - 20 x 20 x 100 mm',(#5878));
#5886=PRODUCT('Hex Bolt - M8x40','Hex Bolt - M8x40','Hex Bolt - M8x40',
(#5878));
#5887=PRODUCT('Swivel arm guide assembly',
'Swivel arm guide assembly','Swivel arm guide assembly',(#5878));
#5888=PRODUCT('Swivel guide arm','Swivel guide arm','Swivel guide arm',
(#5878));
#5889=PRODUCT('Guide contact pad','Guide contact pad',
'Guide contact pad',(#5878));
#5890=PRODUCT('Cap Screw - M4x16','Cap Screw - M4x16',
'Cap Screw - M4x16',(#5878));
#5891=PRODUCT('Flat Washer - M8','Flat Washer - M8','Flat Washer - M8',
(#5878));
#5892=PRODUCT('Hex Nut - M8','Hex Nut - M8','Hex Nut - M8',(#5878));
#5893=PRODUCT('Captive-nut hand knob','Captive-nut hand knob',
'Captive-nut hand knob',(#5878));
#5894=PRESENTATION_STYLE_ASSIGNMENT((#5898));
#5895=PRESENTATION_STYLE_ASSIGNMENT((#5899));
#5896=PRESENTATION_STYLE_ASSIGNMENT((#5900));
#5897=PRESENTATION_STYLE_ASSIGNMENT((#5901));
#5898=SURFACE_STYLE_USAGE(.BOTH.,#5902);
#5899=SURFACE_STYLE_USAGE(.BOTH.,#5903);
#5900=SURFACE_STYLE_USAGE(.BOTH.,#5904);
#5901=SURFACE_STYLE_USAGE(.BOTH.,#5905);
#5902=SURFACE_SIDE_STYLE('',(#5906));
#5903=SURFACE_SIDE_STYLE('',(#5907));
#5904=SURFACE_SIDE_STYLE('',(#5908));
#5905=SURFACE_SIDE_STYLE('',(#5909));
#5906=SURFACE_STYLE_FILL_AREA(#5910);
#5907=SURFACE_STYLE_FILL_AREA(#5911);
#5908=SURFACE_STYLE_FILL_AREA(#5912);
#5909=SURFACE_STYLE_FILL_AREA(#5913);
#5910=FILL_AREA_STYLE('Steel - Satin',(#5914));
#5911=FILL_AREA_STYLE('CAD Library Painted - Steel gray',(#5915));
#5912=FILL_AREA_STYLE('CAD Library Painted - Engineering blue',(#5916));
#5913=FILL_AREA_STYLE('CAD Library Painted - Graphite',(#5917));
#5914=FILL_AREA_STYLE_COLOUR('Steel - Satin',#5918);
#5915=FILL_AREA_STYLE_COLOUR('CAD Library Painted - Steel gray',#5919);
#5916=FILL_AREA_STYLE_COLOUR('CAD Library Painted - Engineering blue',#5920);
#5917=FILL_AREA_STYLE_COLOUR('CAD Library Painted - Graphite',#5921);
#5918=COLOUR_RGB('Steel - Satin',0.627450980392157,0.627450980392157,0.627450980392157);
#5919=COLOUR_RGB('CAD Library Painted - Steel gray',0.592156862745098,0.631372549019608,
0.67843137254902);
#5920=COLOUR_RGB('CAD Library Painted - Engineering blue',0.12156862745098,
0.356862745098039,0.6);
#5921=COLOUR_RGB('CAD Library Painted - Graphite',0.0980392156862745,0.109803921568627,
0.125490196078431);
#5922=COLOUR_RGB('Dark Blue',0.08,0.2,0.34);
#5923=FILL_AREA_STYLE_COLOUR('',#5922);
#5924=FILL_AREA_STYLE('',(#5923));
#5925=SURFACE_STYLE_FILL_AREA(#5924);
#5926=SURFACE_SIDE_STYLE('',(#5925));
#5927=SURFACE_STYLE_USAGE(.BOTH.,#5926);
#5928=PRESENTATION_STYLE_ASSIGNMENT((#5927));
#5929=COLOUR_RGB('Light Blue',0.38,0.62,0.78);
#5930=FILL_AREA_STYLE_COLOUR('',#5929);
#5931=FILL_AREA_STYLE('',(#5930));
#5932=SURFACE_STYLE_FILL_AREA(#5931);
#5933=SURFACE_SIDE_STYLE('',(#5932));
#5934=SURFACE_STYLE_USAGE(.BOTH.,#5933);
#5935=PRESENTATION_STYLE_ASSIGNMENT((#5934));
#5936=COLOUR_RGB('Sky Blue',0.24,0.69,0.87);
#5937=FILL_AREA_STYLE_COLOUR('',#5936);
#5938=FILL_AREA_STYLE('',(#5937));
#5939=SURFACE_STYLE_FILL_AREA(#5938);
#5940=SURFACE_SIDE_STYLE('',(#5939));
#5941=SURFACE_STYLE_USAGE(.BOTH.,#5940);
#5942=PRESENTATION_STYLE_ASSIGNMENT((#5941));
#5943=COLOUR_RGB('Grey',0.48,0.52,0.57);
#5944=FILL_AREA_STYLE_COLOUR('',#5943);
#5945=FILL_AREA_STYLE('',(#5944));
#5946=SURFACE_STYLE_FILL_AREA(#5945);
#5947=SURFACE_SIDE_STYLE('',(#5946));
#5948=SURFACE_STYLE_USAGE(.BOTH.,#5947);
#5949=PRESENTATION_STYLE_ASSIGNMENT((#5948));
#5950=COLOUR_RGB('Black',0.12,0.14,0.17);
#5951=FILL_AREA_STYLE_COLOUR('',#5950);
#5952=FILL_AREA_STYLE('',(#5951));
#5953=SURFACE_STYLE_FILL_AREA(#5952);
#5954=SURFACE_SIDE_STYLE('',(#5953));
#5955=SURFACE_STYLE_USAGE(.BOTH.,#5954);
#5956=PRESENTATION_STYLE_ASSIGNMENT((#5955));
#5957=COLOUR_RGB('Off White',0.89,0.88,0.83);
#5958=FILL_AREA_STYLE_COLOUR('',#5957);
#5959=FILL_AREA_STYLE('',(#5958));
#5960=SURFACE_STYLE_FILL_AREA(#5959);
#5961=SURFACE_SIDE_STYLE('',(#5960));
#5962=SURFACE_STYLE_USAGE(.BOTH.,#5961);
#5963=PRESENTATION_STYLE_ASSIGNMENT((#5962));
ENDSEC;
END-ISO-10303-21;
